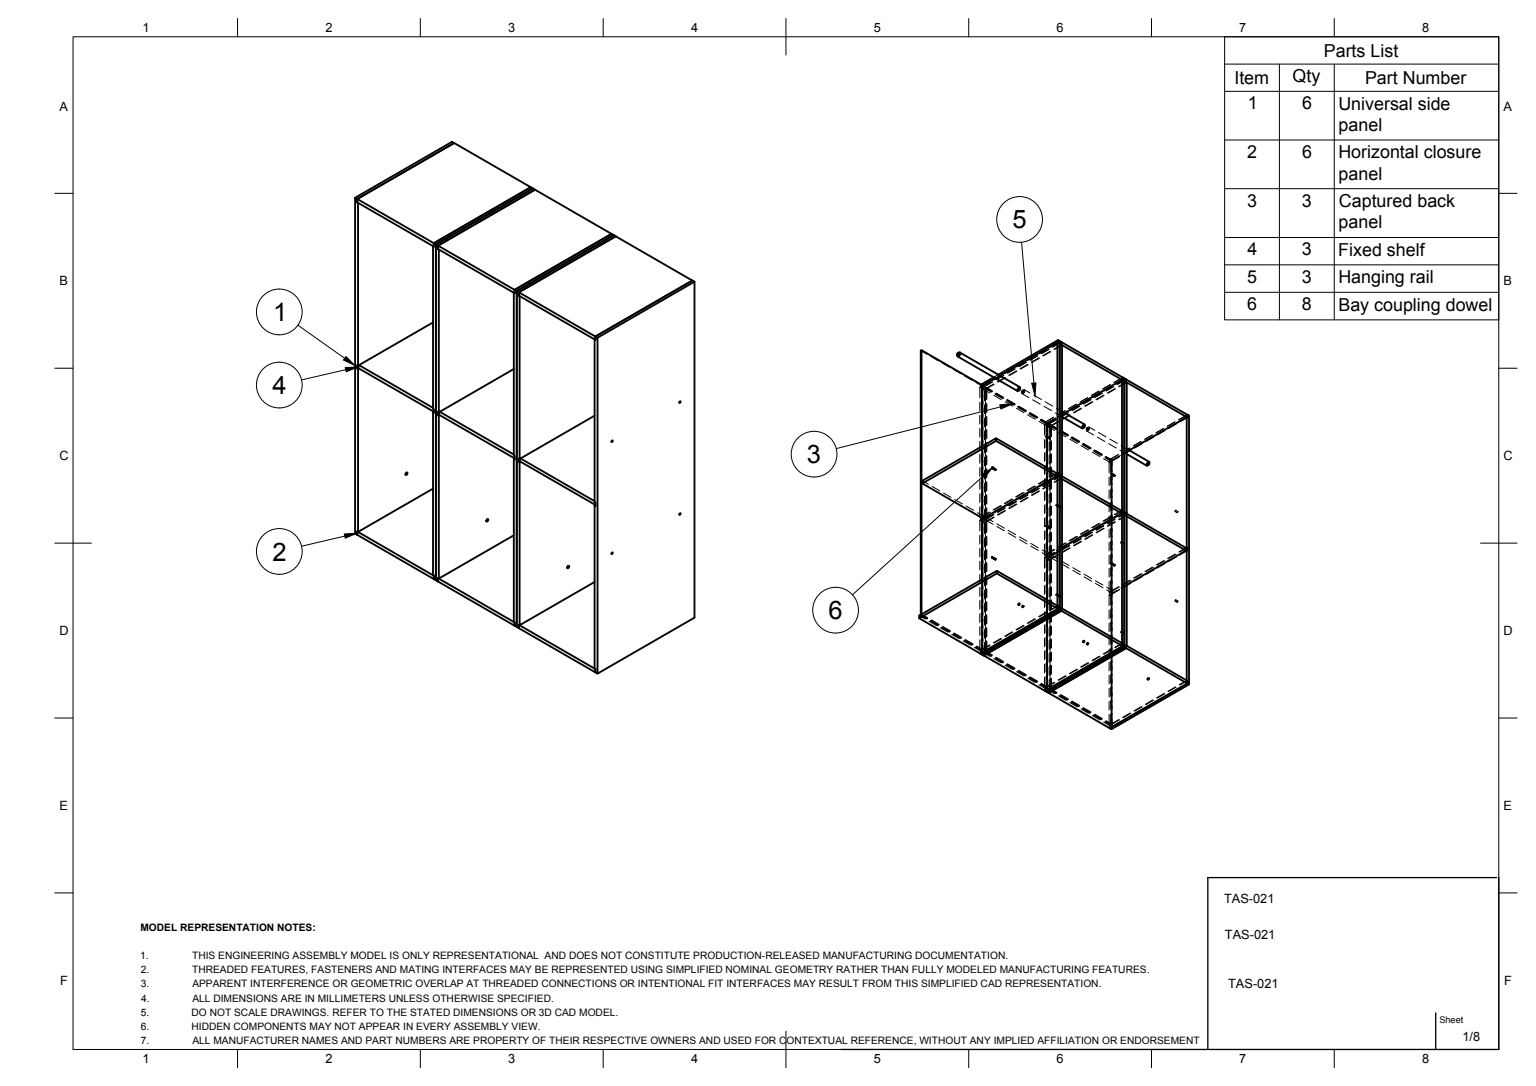
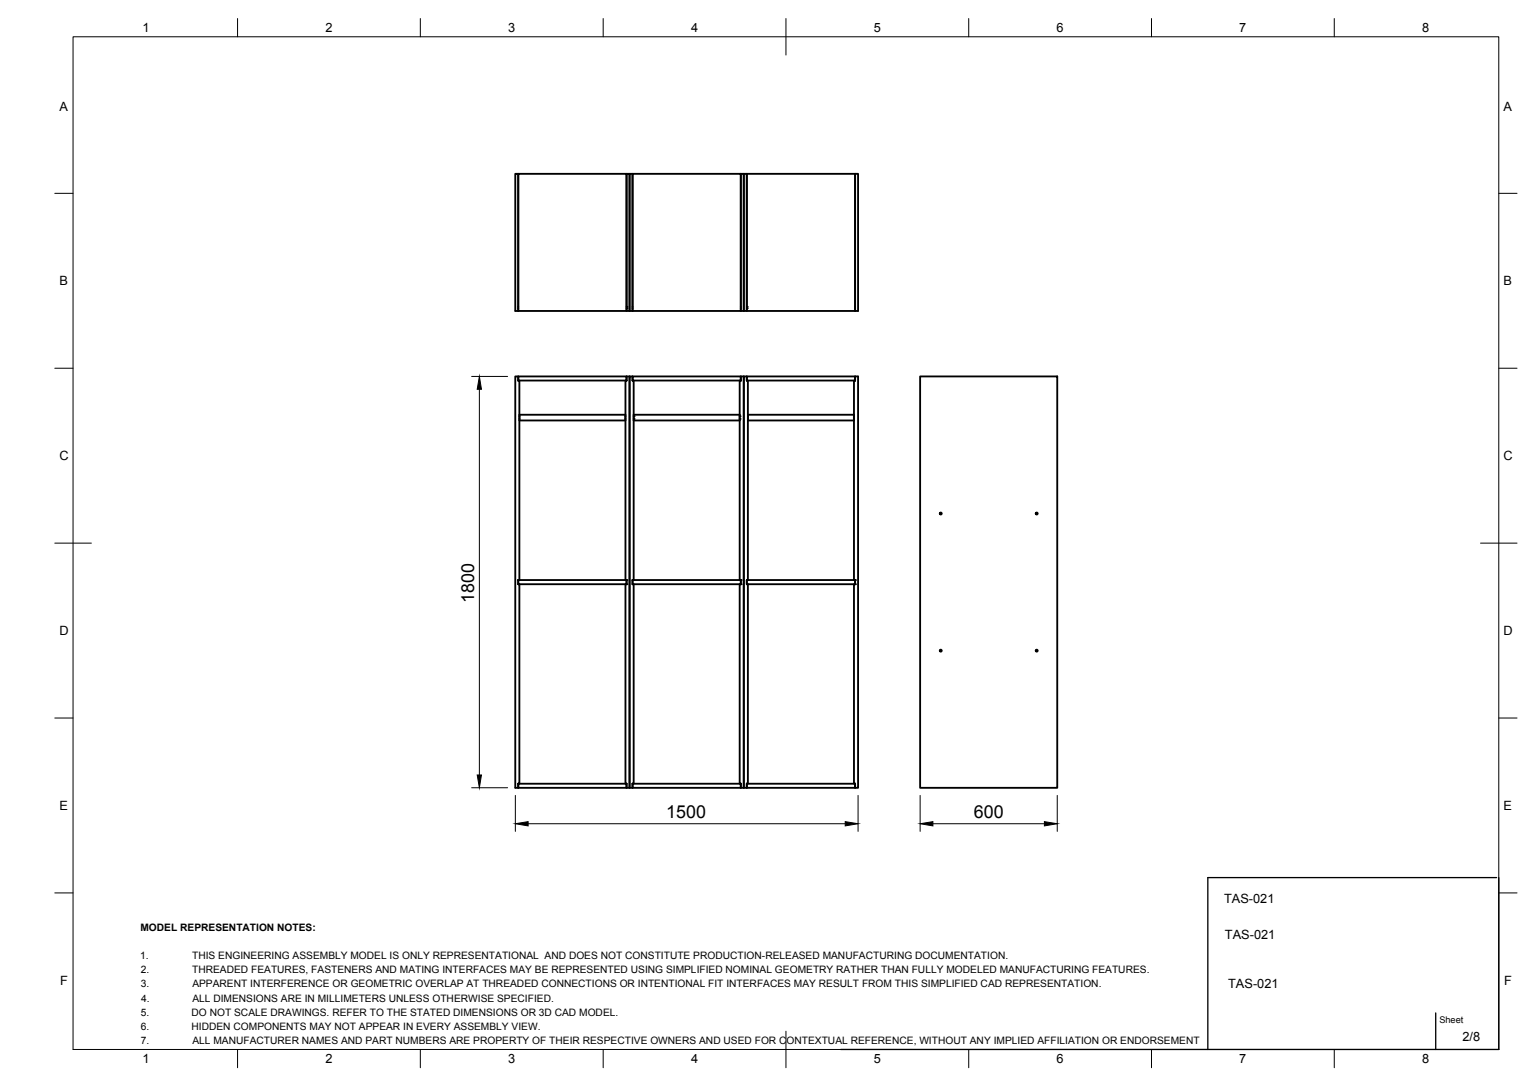
ISO-10303-21;
HEADER;
/* Generated by software containing ST-Developer
 * from STEP Tools, Inc. (www.steptools.com) 
 */

FILE_DESCRIPTION(
/* description */ (''),
/* implementation_level */ '2;1');

FILE_NAME(
/* name */ 'TAS-021.step',
/* time_stamp */ '2026-11-15T17:48:08-08:00',
/* author */ (''),
/* organization */ (''),
/* preprocessor_version */ 'ST-DEVELOPER v20.2',
/* originating_system */ 'Autodesk Translation Framework v15.17.0.0',
/* authorisation */ '');

FILE_SCHEMA (('AUTOMOTIVE_DESIGN { 1 0 10303 214 3 1 1 }'));
ENDSEC;

DATA;
#10=MECHANICAL_DESIGN_GEOMETRIC_PRESENTATION_REPRESENTATION('',(#139,#140,
#141,#142,#143,#144),#2097);
#11=ITEM_DEFINED_TRANSFORMATION($,$,#1267,#1359);
#12=ITEM_DEFINED_TRANSFORMATION($,$,#1314,#1360);
#13=ITEM_DEFINED_TRANSFORMATION($,$,#1325,#1361);
#14=ITEM_DEFINED_TRANSFORMATION($,$,#1332,#1362);
#15=ITEM_DEFINED_TRANSFORMATION($,$,#1339,#1363);
#16=ITEM_DEFINED_TRANSFORMATION($,$,#1353,#1364);
#17=ITEM_DEFINED_TRANSFORMATION($,$,#1267,#1365);
#18=ITEM_DEFINED_TRANSFORMATION($,$,#1314,#1366);
#19=ITEM_DEFINED_TRANSFORMATION($,$,#1267,#1367);
#20=ITEM_DEFINED_TRANSFORMATION($,$,#1267,#1368);
#21=ITEM_DEFINED_TRANSFORMATION($,$,#1314,#1369);
#22=ITEM_DEFINED_TRANSFORMATION($,$,#1314,#1370);
#23=ITEM_DEFINED_TRANSFORMATION($,$,#1325,#1371);
#24=ITEM_DEFINED_TRANSFORMATION($,$,#1332,#1372);
#25=ITEM_DEFINED_TRANSFORMATION($,$,#1339,#1373);
#26=ITEM_DEFINED_TRANSFORMATION($,$,#1267,#1374);
#27=ITEM_DEFINED_TRANSFORMATION($,$,#1267,#1375);
#28=ITEM_DEFINED_TRANSFORMATION($,$,#1314,#1376);
#29=ITEM_DEFINED_TRANSFORMATION($,$,#1314,#1377);
#30=ITEM_DEFINED_TRANSFORMATION($,$,#1325,#1378);
#31=ITEM_DEFINED_TRANSFORMATION($,$,#1332,#1379);
#32=ITEM_DEFINED_TRANSFORMATION($,$,#1339,#1380);
#33=ITEM_DEFINED_TRANSFORMATION($,$,#1353,#1381);
#34=ITEM_DEFINED_TRANSFORMATION($,$,#1353,#1382);
#35=ITEM_DEFINED_TRANSFORMATION($,$,#1353,#1383);
#36=ITEM_DEFINED_TRANSFORMATION($,$,#1353,#1384);
#37=ITEM_DEFINED_TRANSFORMATION($,$,#1353,#1385);
#38=ITEM_DEFINED_TRANSFORMATION($,$,#1353,#1386);
#39=ITEM_DEFINED_TRANSFORMATION($,$,#1353,#1387);
#40=(
REPRESENTATION_RELATIONSHIP($,$,#2146,#2145)
REPRESENTATION_RELATIONSHIP_WITH_TRANSFORMATION(#11)
SHAPE_REPRESENTATION_RELATIONSHIP()
);
#41=(
REPRESENTATION_RELATIONSHIP($,$,#2147,#2145)
REPRESENTATION_RELATIONSHIP_WITH_TRANSFORMATION(#12)
SHAPE_REPRESENTATION_RELATIONSHIP()
);
#42=(
REPRESENTATION_RELATIONSHIP($,$,#2148,#2145)
REPRESENTATION_RELATIONSHIP_WITH_TRANSFORMATION(#13)
SHAPE_REPRESENTATION_RELATIONSHIP()
);
#43=(
REPRESENTATION_RELATIONSHIP($,$,#2149,#2145)
REPRESENTATION_RELATIONSHIP_WITH_TRANSFORMATION(#14)
SHAPE_REPRESENTATION_RELATIONSHIP()
);
#44=(
REPRESENTATION_RELATIONSHIP($,$,#2150,#2145)
REPRESENTATION_RELATIONSHIP_WITH_TRANSFORMATION(#15)
SHAPE_REPRESENTATION_RELATIONSHIP()
);
#45=(
REPRESENTATION_RELATIONSHIP($,$,#2151,#2145)
REPRESENTATION_RELATIONSHIP_WITH_TRANSFORMATION(#16)
SHAPE_REPRESENTATION_RELATIONSHIP()
);
#46=(
REPRESENTATION_RELATIONSHIP($,$,#2146,#2145)
REPRESENTATION_RELATIONSHIP_WITH_TRANSFORMATION(#17)
SHAPE_REPRESENTATION_RELATIONSHIP()
);
#47=(
REPRESENTATION_RELATIONSHIP($,$,#2147,#2145)
REPRESENTATION_RELATIONSHIP_WITH_TRANSFORMATION(#18)
SHAPE_REPRESENTATION_RELATIONSHIP()
);
#48=(
REPRESENTATION_RELATIONSHIP($,$,#2146,#2145)
REPRESENTATION_RELATIONSHIP_WITH_TRANSFORMATION(#19)
SHAPE_REPRESENTATION_RELATIONSHIP()
);
#49=(
REPRESENTATION_RELATIONSHIP($,$,#2146,#2145)
REPRESENTATION_RELATIONSHIP_WITH_TRANSFORMATION(#20)
SHAPE_REPRESENTATION_RELATIONSHIP()
);
#50=(
REPRESENTATION_RELATIONSHIP($,$,#2147,#2145)
REPRESENTATION_RELATIONSHIP_WITH_TRANSFORMATION(#21)
SHAPE_REPRESENTATION_RELATIONSHIP()
);
#51=(
REPRESENTATION_RELATIONSHIP($,$,#2147,#2145)
REPRESENTATION_RELATIONSHIP_WITH_TRANSFORMATION(#22)
SHAPE_REPRESENTATION_RELATIONSHIP()
);
#52=(
REPRESENTATION_RELATIONSHIP($,$,#2148,#2145)
REPRESENTATION_RELATIONSHIP_WITH_TRANSFORMATION(#23)
SHAPE_REPRESENTATION_RELATIONSHIP()
);
#53=(
REPRESENTATION_RELATIONSHIP($,$,#2149,#2145)
REPRESENTATION_RELATIONSHIP_WITH_TRANSFORMATION(#24)
SHAPE_REPRESENTATION_RELATIONSHIP()
);
#54=(
REPRESENTATION_RELATIONSHIP($,$,#2150,#2145)
REPRESENTATION_RELATIONSHIP_WITH_TRANSFORMATION(#25)
SHAPE_REPRESENTATION_RELATIONSHIP()
);
#55=(
REPRESENTATION_RELATIONSHIP($,$,#2146,#2145)
REPRESENTATION_RELATIONSHIP_WITH_TRANSFORMATION(#26)
SHAPE_REPRESENTATION_RELATIONSHIP()
);
#56=(
REPRESENTATION_RELATIONSHIP($,$,#2146,#2145)
REPRESENTATION_RELATIONSHIP_WITH_TRANSFORMATION(#27)
SHAPE_REPRESENTATION_RELATIONSHIP()
);
#57=(
REPRESENTATION_RELATIONSHIP($,$,#2147,#2145)
REPRESENTATION_RELATIONSHIP_WITH_TRANSFORMATION(#28)
SHAPE_REPRESENTATION_RELATIONSHIP()
);
#58=(
REPRESENTATION_RELATIONSHIP($,$,#2147,#2145)
REPRESENTATION_RELATIONSHIP_WITH_TRANSFORMATION(#29)
SHAPE_REPRESENTATION_RELATIONSHIP()
);
#59=(
REPRESENTATION_RELATIONSHIP($,$,#2148,#2145)
REPRESENTATION_RELATIONSHIP_WITH_TRANSFORMATION(#30)
SHAPE_REPRESENTATION_RELATIONSHIP()
);
#60=(
REPRESENTATION_RELATIONSHIP($,$,#2149,#2145)
REPRESENTATION_RELATIONSHIP_WITH_TRANSFORMATION(#31)
SHAPE_REPRESENTATION_RELATIONSHIP()
);
#61=(
REPRESENTATION_RELATIONSHIP($,$,#2150,#2145)
REPRESENTATION_RELATIONSHIP_WITH_TRANSFORMATION(#32)
SHAPE_REPRESENTATION_RELATIONSHIP()
);
#62=(
REPRESENTATION_RELATIONSHIP($,$,#2151,#2145)
REPRESENTATION_RELATIONSHIP_WITH_TRANSFORMATION(#33)
SHAPE_REPRESENTATION_RELATIONSHIP()
);
#63=(
REPRESENTATION_RELATIONSHIP($,$,#2151,#2145)
REPRESENTATION_RELATIONSHIP_WITH_TRANSFORMATION(#34)
SHAPE_REPRESENTATION_RELATIONSHIP()
);
#64=(
REPRESENTATION_RELATIONSHIP($,$,#2151,#2145)
REPRESENTATION_RELATIONSHIP_WITH_TRANSFORMATION(#35)
SHAPE_REPRESENTATION_RELATIONSHIP()
);
#65=(
REPRESENTATION_RELATIONSHIP($,$,#2151,#2145)
REPRESENTATION_RELATIONSHIP_WITH_TRANSFORMATION(#36)
SHAPE_REPRESENTATION_RELATIONSHIP()
);
#66=(
REPRESENTATION_RELATIONSHIP($,$,#2151,#2145)
REPRESENTATION_RELATIONSHIP_WITH_TRANSFORMATION(#37)
SHAPE_REPRESENTATION_RELATIONSHIP()
);
#67=(
REPRESENTATION_RELATIONSHIP($,$,#2151,#2145)
REPRESENTATION_RELATIONSHIP_WITH_TRANSFORMATION(#38)
SHAPE_REPRESENTATION_RELATIONSHIP()
);
#68=(
REPRESENTATION_RELATIONSHIP($,$,#2151,#2145)
REPRESENTATION_RELATIONSHIP_WITH_TRANSFORMATION(#39)
SHAPE_REPRESENTATION_RELATIONSHIP()
);
#69=CONTEXT_DEPENDENT_SHAPE_REPRESENTATION(#40,#2116);
#70=CONTEXT_DEPENDENT_SHAPE_REPRESENTATION(#41,#2117);
#71=CONTEXT_DEPENDENT_SHAPE_REPRESENTATION(#42,#2118);
#72=CONTEXT_DEPENDENT_SHAPE_REPRESENTATION(#43,#2119);
#73=CONTEXT_DEPENDENT_SHAPE_REPRESENTATION(#44,#2120);
#74=CONTEXT_DEPENDENT_SHAPE_REPRESENTATION(#45,#2121);
#75=CONTEXT_DEPENDENT_SHAPE_REPRESENTATION(#46,#2122);
#76=CONTEXT_DEPENDENT_SHAPE_REPRESENTATION(#47,#2123);
#77=CONTEXT_DEPENDENT_SHAPE_REPRESENTATION(#48,#2124);
#78=CONTEXT_DEPENDENT_SHAPE_REPRESENTATION(#49,#2125);
#79=CONTEXT_DEPENDENT_SHAPE_REPRESENTATION(#50,#2126);
#80=CONTEXT_DEPENDENT_SHAPE_REPRESENTATION(#51,#2127);
#81=CONTEXT_DEPENDENT_SHAPE_REPRESENTATION(#52,#2128);
#82=CONTEXT_DEPENDENT_SHAPE_REPRESENTATION(#53,#2129);
#83=CONTEXT_DEPENDENT_SHAPE_REPRESENTATION(#54,#2130);
#84=CONTEXT_DEPENDENT_SHAPE_REPRESENTATION(#55,#2131);
#85=CONTEXT_DEPENDENT_SHAPE_REPRESENTATION(#56,#2132);
#86=CONTEXT_DEPENDENT_SHAPE_REPRESENTATION(#57,#2133);
#87=CONTEXT_DEPENDENT_SHAPE_REPRESENTATION(#58,#2134);
#88=CONTEXT_DEPENDENT_SHAPE_REPRESENTATION(#59,#2135);
#89=CONTEXT_DEPENDENT_SHAPE_REPRESENTATION(#60,#2136);
#90=CONTEXT_DEPENDENT_SHAPE_REPRESENTATION(#61,#2137);
#91=CONTEXT_DEPENDENT_SHAPE_REPRESENTATION(#62,#2138);
#92=CONTEXT_DEPENDENT_SHAPE_REPRESENTATION(#63,#2139);
#93=CONTEXT_DEPENDENT_SHAPE_REPRESENTATION(#64,#2140);
#94=CONTEXT_DEPENDENT_SHAPE_REPRESENTATION(#65,#2141);
#95=CONTEXT_DEPENDENT_SHAPE_REPRESENTATION(#66,#2142);
#96=CONTEXT_DEPENDENT_SHAPE_REPRESENTATION(#67,#2143);
#97=CONTEXT_DEPENDENT_SHAPE_REPRESENTATION(#68,#2144);
#98=NEXT_ASSEMBLY_USAGE_OCCURRENCE('Universal side panel:1',
'Universal side panel:1','Universal side panel:1',#2153,#2154,
'Universal side panel:1');
#99=NEXT_ASSEMBLY_USAGE_OCCURRENCE('Horizontal closure panel:1',
'Horizontal closure panel:1','Horizontal closure panel:1',#2153,#2155,
'Horizontal closure panel:1');
#100=NEXT_ASSEMBLY_USAGE_OCCURRENCE('Captured back panel:1',
'Captured back panel:1','Captured back panel:1',#2153,#2156,
'Captured back panel:1');
#101=NEXT_ASSEMBLY_USAGE_OCCURRENCE('Fixed shelf:1','Fixed shelf:1',
'Fixed shelf:1',#2153,#2157,'Fixed shelf:1');
#102=NEXT_ASSEMBLY_USAGE_OCCURRENCE('Hanging rail:1','Hanging rail:1',
'Hanging rail:1',#2153,#2158,'Hanging rail:1');
#103=NEXT_ASSEMBLY_USAGE_OCCURRENCE('Bay coupling dowel:1',
'Bay coupling dowel:1','Bay coupling dowel:1',#2153,#2159,
'Bay coupling dowel:1');
#104=NEXT_ASSEMBLY_USAGE_OCCURRENCE('Universal side panel:2',
'Universal side panel:2','Universal side panel:2',#2153,#2154,
'Universal side panel:2');
#105=NEXT_ASSEMBLY_USAGE_OCCURRENCE('Horizontal closure panel:2',
'Horizontal closure panel:2','Horizontal closure panel:2',#2153,#2155,
'Horizontal closure panel:2');
#106=NEXT_ASSEMBLY_USAGE_OCCURRENCE('Universal side panel:3',
'Universal side panel:3','Universal side panel:3',#2153,#2154,
'Universal side panel:3');
#107=NEXT_ASSEMBLY_USAGE_OCCURRENCE('Universal side panel:4',
'Universal side panel:4','Universal side panel:4',#2153,#2154,
'Universal side panel:4');
#108=NEXT_ASSEMBLY_USAGE_OCCURRENCE('Horizontal closure panel:3',
'Horizontal closure panel:3','Horizontal closure panel:3',#2153,#2155,
'Horizontal closure panel:3');
#109=NEXT_ASSEMBLY_USAGE_OCCURRENCE('Horizontal closure panel:4',
'Horizontal closure panel:4','Horizontal closure panel:4',#2153,#2155,
'Horizontal closure panel:4');
#110=NEXT_ASSEMBLY_USAGE_OCCURRENCE('Captured back panel:2',
'Captured back panel:2','Captured back panel:2',#2153,#2156,
'Captured back panel:2');
#111=NEXT_ASSEMBLY_USAGE_OCCURRENCE('Fixed shelf:2','Fixed shelf:2',
'Fixed shelf:2',#2153,#2157,'Fixed shelf:2');
#112=NEXT_ASSEMBLY_USAGE_OCCURRENCE('Hanging rail:2','Hanging rail:2',
'Hanging rail:2',#2153,#2158,'Hanging rail:2');
#113=NEXT_ASSEMBLY_USAGE_OCCURRENCE('Universal side panel:5',
'Universal side panel:5','Universal side panel:5',#2153,#2154,
'Universal side panel:5');
#114=NEXT_ASSEMBLY_USAGE_OCCURRENCE('Universal side panel:6',
'Universal side panel:6','Universal side panel:6',#2153,#2154,
'Universal side panel:6');
#115=NEXT_ASSEMBLY_USAGE_OCCURRENCE('Horizontal closure panel:5',
'Horizontal closure panel:5','Horizontal closure panel:5',#2153,#2155,
'Horizontal closure panel:5');
#116=NEXT_ASSEMBLY_USAGE_OCCURRENCE('Horizontal closure panel:6',
'Horizontal closure panel:6','Horizontal closure panel:6',#2153,#2155,
'Horizontal closure panel:6');
#117=NEXT_ASSEMBLY_USAGE_OCCURRENCE('Captured back panel:3',
'Captured back panel:3','Captured back panel:3',#2153,#2156,
'Captured back panel:3');
#118=NEXT_ASSEMBLY_USAGE_OCCURRENCE('Fixed shelf:3','Fixed shelf:3',
'Fixed shelf:3',#2153,#2157,'Fixed shelf:3');
#119=NEXT_ASSEMBLY_USAGE_OCCURRENCE('Hanging rail:3','Hanging rail:3',
'Hanging rail:3',#2153,#2158,'Hanging rail:3');
#120=NEXT_ASSEMBLY_USAGE_OCCURRENCE('Bay coupling dowel:2',
'Bay coupling dowel:2','Bay coupling dowel:2',#2153,#2159,
'Bay coupling dowel:2');
#121=NEXT_ASSEMBLY_USAGE_OCCURRENCE('Bay coupling dowel:3',
'Bay coupling dowel:3','Bay coupling dowel:3',#2153,#2159,
'Bay coupling dowel:3');
#122=NEXT_ASSEMBLY_USAGE_OCCURRENCE('Bay coupling dowel:4',
'Bay coupling dowel:4','Bay coupling dowel:4',#2153,#2159,
'Bay coupling dowel:4');
#123=NEXT_ASSEMBLY_USAGE_OCCURRENCE('Bay coupling dowel:5',
'Bay coupling dowel:5','Bay coupling dowel:5',#2153,#2159,
'Bay coupling dowel:5');
#124=NEXT_ASSEMBLY_USAGE_OCCURRENCE('Bay coupling dowel:6',
'Bay coupling dowel:6','Bay coupling dowel:6',#2153,#2159,
'Bay coupling dowel:6');
#125=NEXT_ASSEMBLY_USAGE_OCCURRENCE('Bay coupling dowel:7',
'Bay coupling dowel:7','Bay coupling dowel:7',#2153,#2159,
'Bay coupling dowel:7');
#126=NEXT_ASSEMBLY_USAGE_OCCURRENCE('Bay coupling dowel:8',
'Bay coupling dowel:8','Bay coupling dowel:8',#2153,#2159,
'Bay coupling dowel:8');
#127=SHAPE_REPRESENTATION_RELATIONSHIP('SRR','None',#2146,#133);
#128=SHAPE_REPRESENTATION_RELATIONSHIP('SRR','None',#2147,#134);
#129=SHAPE_REPRESENTATION_RELATIONSHIP('SRR','None',#2148,#135);
#130=SHAPE_REPRESENTATION_RELATIONSHIP('SRR','None',#2149,#136);
#131=SHAPE_REPRESENTATION_RELATIONSHIP('SRR','None',#2150,#137);
#132=SHAPE_REPRESENTATION_RELATIONSHIP('SRR','None',#2151,#138);
#133=ADVANCED_BREP_SHAPE_REPRESENTATION('',(#145),#2091);
#134=ADVANCED_BREP_SHAPE_REPRESENTATION('',(#146),#2092);
#135=ADVANCED_BREP_SHAPE_REPRESENTATION('',(#147),#2093);
#136=ADVANCED_BREP_SHAPE_REPRESENTATION('',(#148),#2094);
#137=ADVANCED_BREP_SHAPE_REPRESENTATION('',(#149),#2095);
#138=ADVANCED_BREP_SHAPE_REPRESENTATION('',(#150),#2096);
#139=STYLED_ITEM('',(#2185),#145);
#140=STYLED_ITEM('',(#2186),#146);
#141=STYLED_ITEM('',(#2187),#147);
#142=STYLED_ITEM('',(#2188),#148);
#143=STYLED_ITEM('',(#2189),#149);
#144=STYLED_ITEM('',(#2190),#150);
#145=MANIFOLD_SOLID_BREP('Body1',#1193);
#146=MANIFOLD_SOLID_BREP('Body1',#1194);
#147=MANIFOLD_SOLID_BREP('Body1',#1195);
#148=MANIFOLD_SOLID_BREP('Body1',#1196);
#149=MANIFOLD_SOLID_BREP('Body1',#1197);
#150=MANIFOLD_SOLID_BREP('Body1',#1198);
#151=FACE_BOUND('',#301,.T.);
#152=FACE_BOUND('',#308,.T.);
#153=FACE_BOUND('',#316,.T.);
#154=FACE_BOUND('',#317,.T.);
#155=FACE_BOUND('',#318,.T.);
#156=FACE_BOUND('',#319,.T.);
#157=FACE_BOUND('',#349,.T.);
#158=FACE_BOUND('',#351,.T.);
#159=PLANE('',#1271);
#160=PLANE('',#1275);
#161=PLANE('',#1279);
#162=PLANE('',#1283);
#163=PLANE('',#1287);
#164=PLANE('',#1291);
#165=PLANE('',#1292);
#166=PLANE('',#1293);
#167=PLANE('',#1294);
#168=PLANE('',#1295);
#169=PLANE('',#1296);
#170=PLANE('',#1297);
#171=PLANE('',#1298);
#172=PLANE('',#1299);
#173=PLANE('',#1300);
#174=PLANE('',#1301);
#175=PLANE('',#1302);
#176=PLANE('',#1303);
#177=PLANE('',#1304);
#178=PLANE('',#1305);
#179=PLANE('',#1306);
#180=PLANE('',#1307);
#181=PLANE('',#1308);
#182=PLANE('',#1309);
#183=PLANE('',#1310);
#184=PLANE('',#1311);
#185=PLANE('',#1312);
#186=PLANE('',#1313);
#187=PLANE('',#1315);
#188=PLANE('',#1316);
#189=PLANE('',#1317);
#190=PLANE('',#1318);
#191=PLANE('',#1319);
#192=PLANE('',#1320);
#193=PLANE('',#1321);
#194=PLANE('',#1322);
#195=PLANE('',#1323);
#196=PLANE('',#1324);
#197=PLANE('',#1326);
#198=PLANE('',#1327);
#199=PLANE('',#1328);
#200=PLANE('',#1329);
#201=PLANE('',#1330);
#202=PLANE('',#1331);
#203=PLANE('',#1333);
#204=PLANE('',#1334);
#205=PLANE('',#1335);
#206=PLANE('',#1336);
#207=PLANE('',#1337);
#208=PLANE('',#1338);
#209=PLANE('',#1343);
#210=PLANE('',#1347);
#211=PLANE('',#1351);
#212=PLANE('',#1352);
#213=PLANE('',#1357);
#214=PLANE('',#1358);
#215=FACE_OUTER_BOUND('',#281,.T.);
#216=FACE_OUTER_BOUND('',#282,.T.);
#217=FACE_OUTER_BOUND('',#283,.T.);
#218=FACE_OUTER_BOUND('',#284,.T.);
#219=FACE_OUTER_BOUND('',#285,.T.);
#220=FACE_OUTER_BOUND('',#286,.T.);
#221=FACE_OUTER_BOUND('',#287,.T.);
#222=FACE_OUTER_BOUND('',#288,.T.);
#223=FACE_OUTER_BOUND('',#289,.T.);
#224=FACE_OUTER_BOUND('',#290,.T.);
#225=FACE_OUTER_BOUND('',#291,.T.);
#226=FACE_OUTER_BOUND('',#292,.T.);
#227=FACE_OUTER_BOUND('',#293,.T.);
#228=FACE_OUTER_BOUND('',#294,.T.);
#229=FACE_OUTER_BOUND('',#295,.T.);
#230=FACE_OUTER_BOUND('',#296,.T.);
#231=FACE_OUTER_BOUND('',#297,.T.);
#232=FACE_OUTER_BOUND('',#298,.T.);
#233=FACE_OUTER_BOUND('',#299,.T.);
#234=FACE_OUTER_BOUND('',#300,.T.);
#235=FACE_OUTER_BOUND('',#302,.T.);
#236=FACE_OUTER_BOUND('',#303,.T.);
#237=FACE_OUTER_BOUND('',#304,.T.);
#238=FACE_OUTER_BOUND('',#305,.T.);
#239=FACE_OUTER_BOUND('',#306,.T.);
#240=FACE_OUTER_BOUND('',#307,.T.);
#241=FACE_OUTER_BOUND('',#309,.T.);
#242=FACE_OUTER_BOUND('',#310,.T.);
#243=FACE_OUTER_BOUND('',#311,.T.);
#244=FACE_OUTER_BOUND('',#312,.T.);
#245=FACE_OUTER_BOUND('',#313,.T.);
#246=FACE_OUTER_BOUND('',#314,.T.);
#247=FACE_OUTER_BOUND('',#315,.T.);
#248=FACE_OUTER_BOUND('',#320,.T.);
#249=FACE_OUTER_BOUND('',#321,.T.);
#250=FACE_OUTER_BOUND('',#322,.T.);
#251=FACE_OUTER_BOUND('',#323,.T.);
#252=FACE_OUTER_BOUND('',#324,.T.);
#253=FACE_OUTER_BOUND('',#325,.T.);
#254=FACE_OUTER_BOUND('',#326,.T.);
#255=FACE_OUTER_BOUND('',#327,.T.);
#256=FACE_OUTER_BOUND('',#328,.T.);
#257=FACE_OUTER_BOUND('',#329,.T.);
#258=FACE_OUTER_BOUND('',#330,.T.);
#259=FACE_OUTER_BOUND('',#331,.T.);
#260=FACE_OUTER_BOUND('',#332,.T.);
#261=FACE_OUTER_BOUND('',#333,.T.);
#262=FACE_OUTER_BOUND('',#334,.T.);
#263=FACE_OUTER_BOUND('',#335,.T.);
#264=FACE_OUTER_BOUND('',#336,.T.);
#265=FACE_OUTER_BOUND('',#337,.T.);
#266=FACE_OUTER_BOUND('',#338,.T.);
#267=FACE_OUTER_BOUND('',#339,.T.);
#268=FACE_OUTER_BOUND('',#340,.T.);
#269=FACE_OUTER_BOUND('',#341,.T.);
#270=FACE_OUTER_BOUND('',#342,.T.);
#271=FACE_OUTER_BOUND('',#343,.T.);
#272=FACE_OUTER_BOUND('',#344,.T.);
#273=FACE_OUTER_BOUND('',#345,.T.);
#274=FACE_OUTER_BOUND('',#346,.T.);
#275=FACE_OUTER_BOUND('',#347,.T.);
#276=FACE_OUTER_BOUND('',#348,.T.);
#277=FACE_OUTER_BOUND('',#350,.T.);
#278=FACE_OUTER_BOUND('',#352,.T.);
#279=FACE_OUTER_BOUND('',#353,.T.);
#280=FACE_OUTER_BOUND('',#354,.T.);
#281=EDGE_LOOP('',(#841,#842,#843,#844));
#282=EDGE_LOOP('',(#845));
#283=EDGE_LOOP('',(#846,#847,#848,#849));
#284=EDGE_LOOP('',(#850));
#285=EDGE_LOOP('',(#851,#852,#853,#854));
#286=EDGE_LOOP('',(#855));
#287=EDGE_LOOP('',(#856,#857,#858,#859));
#288=EDGE_LOOP('',(#860));
#289=EDGE_LOOP('',(#861,#862,#863,#864));
#290=EDGE_LOOP('',(#865));
#291=EDGE_LOOP('',(#866,#867,#868,#869));
#292=EDGE_LOOP('',(#870));
#293=EDGE_LOOP('',(#871,#872,#873,#874));
#294=EDGE_LOOP('',(#875,#876,#877,#878));
#295=EDGE_LOOP('',(#879,#880,#881,#882));
#296=EDGE_LOOP('',(#883,#884,#885,#886));
#297=EDGE_LOOP('',(#887,#888,#889,#890,#891,#892,#893,#894,#895,#896,#897,
#898,#899,#900,#901,#902,#903,#904,#905,#906));
#298=EDGE_LOOP('',(#907,#908,#909,#910));
#299=EDGE_LOOP('',(#911,#912,#913,#914));
#300=EDGE_LOOP('',(#915,#916,#917,#918));
#301=EDGE_LOOP('',(#919));
#302=EDGE_LOOP('',(#920,#921,#922,#923));
#303=EDGE_LOOP('',(#924,#925,#926,#927));
#304=EDGE_LOOP('',(#928,#929,#930,#931));
#305=EDGE_LOOP('',(#932,#933,#934,#935));
#306=EDGE_LOOP('',(#936,#937,#938,#939));
#307=EDGE_LOOP('',(#940,#941,#942,#943));
#308=EDGE_LOOP('',(#944));
#309=EDGE_LOOP('',(#945,#946,#947,#948));
#310=EDGE_LOOP('',(#949,#950,#951,#952));
#311=EDGE_LOOP('',(#953,#954,#955,#956));
#312=EDGE_LOOP('',(#957,#958,#959,#960,#961,#962,#963,#964,#965,#966,#967,
#968));
#313=EDGE_LOOP('',(#969,#970,#971,#972));
#314=EDGE_LOOP('',(#973,#974,#975,#976,#977,#978,#979,#980,#981,#982,#983,
#984));
#315=EDGE_LOOP('',(#985,#986,#987,#988));
#316=EDGE_LOOP('',(#989));
#317=EDGE_LOOP('',(#990));
#318=EDGE_LOOP('',(#991));
#319=EDGE_LOOP('',(#992));
#320=EDGE_LOOP('',(#993,#994,#995,#996));
#321=EDGE_LOOP('',(#997,#998,#999,#1000));
#322=EDGE_LOOP('',(#1001,#1002,#1003,#1004));
#323=EDGE_LOOP('',(#1005,#1006,#1007,#1008));
#324=EDGE_LOOP('',(#1009,#1010,#1011,#1012,#1013,#1014,#1015,#1016));
#325=EDGE_LOOP('',(#1017,#1018,#1019,#1020));
#326=EDGE_LOOP('',(#1021,#1022,#1023,#1024));
#327=EDGE_LOOP('',(#1025,#1026,#1027,#1028));
#328=EDGE_LOOP('',(#1029,#1030,#1031,#1032,#1033,#1034,#1035,#1036));
#329=EDGE_LOOP('',(#1037,#1038,#1039,#1040));
#330=EDGE_LOOP('',(#1041,#1042,#1043,#1044));
#331=EDGE_LOOP('',(#1045,#1046,#1047,#1048));
#332=EDGE_LOOP('',(#1049,#1050,#1051,#1052));
#333=EDGE_LOOP('',(#1053,#1054,#1055,#1056));
#334=EDGE_LOOP('',(#1057,#1058,#1059,#1060));
#335=EDGE_LOOP('',(#1061,#1062,#1063,#1064));
#336=EDGE_LOOP('',(#1065,#1066,#1067,#1068));
#337=EDGE_LOOP('',(#1069,#1070,#1071,#1072));
#338=EDGE_LOOP('',(#1073,#1074,#1075,#1076));
#339=EDGE_LOOP('',(#1077,#1078,#1079,#1080));
#340=EDGE_LOOP('',(#1081,#1082,#1083,#1084));
#341=EDGE_LOOP('',(#1085,#1086,#1087,#1088));
#342=EDGE_LOOP('',(#1089,#1090,#1091,#1092));
#343=EDGE_LOOP('',(#1093,#1094,#1095,#1096));
#344=EDGE_LOOP('',(#1097));
#345=EDGE_LOOP('',(#1098,#1099,#1100,#1101));
#346=EDGE_LOOP('',(#1102));
#347=EDGE_LOOP('',(#1103,#1104,#1105,#1106));
#348=EDGE_LOOP('',(#1107));
#349=EDGE_LOOP('',(#1108));
#350=EDGE_LOOP('',(#1109));
#351=EDGE_LOOP('',(#1110));
#352=EDGE_LOOP('',(#1111,#1112,#1113,#1114));
#353=EDGE_LOOP('',(#1115));
#354=EDGE_LOOP('',(#1116));
#355=LINE('',#1756,#473);
#356=LINE('',#1763,#474);
#357=LINE('',#1770,#475);
#358=LINE('',#1777,#476);
#359=LINE('',#1784,#477);
#360=LINE('',#1791,#478);
#361=LINE('',#1797,#479);
#362=LINE('',#1799,#480);
#363=LINE('',#1801,#481);
#364=LINE('',#1802,#482);
#365=LINE('',#1806,#483);
#366=LINE('',#1808,#484);
#367=LINE('',#1810,#485);
#368=LINE('',#1811,#486);
#369=LINE('',#1815,#487);
#370=LINE('',#1817,#488);
#371=LINE('',#1819,#489);
#372=LINE('',#1820,#490);
#373=LINE('',#1824,#491);
#374=LINE('',#1826,#492);
#375=LINE('',#1828,#493);
#376=LINE('',#1829,#494);
#377=LINE('',#1832,#495);
#378=LINE('',#1834,#496);
#379=LINE('',#1836,#497);
#380=LINE('',#1838,#498);
#381=LINE('',#1839,#499);
#382=LINE('',#1841,#500);
#383=LINE('',#1843,#501);
#384=LINE('',#1844,#502);
#385=LINE('',#1846,#503);
#386=LINE('',#1848,#504);
#387=LINE('',#1850,#505);
#388=LINE('',#1852,#506);
#389=LINE('',#1853,#507);
#390=LINE('',#1855,#508);
#391=LINE('',#1857,#509);
#392=LINE('',#1858,#510);
#393=LINE('',#1861,#511);
#394=LINE('',#1862,#512);
#395=LINE('',#1865,#513);
#396=LINE('',#1866,#514);
#397=LINE('',#1869,#515);
#398=LINE('',#1870,#516);
#399=LINE('',#1873,#517);
#400=LINE('',#1874,#518);
#401=LINE('',#1876,#519);
#402=LINE('',#1878,#520);
#403=LINE('',#1881,#521);
#404=LINE('',#1882,#522);
#405=LINE('',#1885,#523);
#406=LINE('',#1886,#524);
#407=LINE('',#1889,#525);
#408=LINE('',#1890,#526);
#409=LINE('',#1893,#527);
#410=LINE('',#1894,#528);
#411=LINE('',#1896,#529);
#412=LINE('',#1898,#530);
#413=LINE('',#1901,#531);
#414=LINE('',#1903,#532);
#415=LINE('',#1904,#533);
#416=LINE('',#1907,#534);
#417=LINE('',#1908,#535);
#418=LINE('',#1911,#536);
#419=LINE('',#1912,#537);
#420=LINE('',#1914,#538);
#421=LINE('',#1920,#539);
#422=LINE('',#1922,#540);
#423=LINE('',#1924,#541);
#424=LINE('',#1925,#542);
#425=LINE('',#1929,#543);
#426=LINE('',#1931,#544);
#427=LINE('',#1933,#545);
#428=LINE('',#1934,#546);
#429=LINE('',#1936,#547);
#430=LINE('',#1937,#548);
#431=LINE('',#1940,#549);
#432=LINE('',#1942,#550);
#433=LINE('',#1944,#551);
#434=LINE('',#1946,#552);
#435=LINE('',#1947,#553);
#436=LINE('',#1950,#554);
#437=LINE('',#1951,#555);
#438=LINE('',#1954,#556);
#439=LINE('',#1956,#557);
#440=LINE('',#1957,#558);
#441=LINE('',#1960,#559);
#442=LINE('',#1961,#560);
#443=LINE('',#1963,#561);
#444=LINE('',#1964,#562);
#445=LINE('',#1971,#563);
#446=LINE('',#1973,#564);
#447=LINE('',#1975,#565);
#448=LINE('',#1976,#566);
#449=LINE('',#1979,#567);
#450=LINE('',#1981,#568);
#451=LINE('',#1982,#569);
#452=LINE('',#1985,#570);
#453=LINE('',#1987,#571);
#454=LINE('',#1988,#572);
#455=LINE('',#1990,#573);
#456=LINE('',#1991,#574);
#457=LINE('',#1998,#575);
#458=LINE('',#2000,#576);
#459=LINE('',#2002,#577);
#460=LINE('',#2003,#578);
#461=LINE('',#2006,#579);
#462=LINE('',#2008,#580);
#463=LINE('',#2009,#581);
#464=LINE('',#2012,#582);
#465=LINE('',#2014,#583);
#466=LINE('',#2015,#584);
#467=LINE('',#2017,#585);
#468=LINE('',#2018,#586);
#469=LINE('',#2026,#587);
#470=LINE('',#2033,#588);
#471=LINE('',#2040,#589);
#472=LINE('',#2049,#590);
#473=VECTOR('',#1396,0.409999999999997);
#474=VECTOR('',#1405,0.409999999999997);
#475=VECTOR('',#1414,0.409999999999997);
#476=VECTOR('',#1423,0.409999999999997);
#477=VECTOR('',#1432,0.620000000000001);
#478=VECTOR('',#1441,0.620000000000005);
#479=VECTOR('',#1448,1.);
#480=VECTOR('',#1449,1.);
#481=VECTOR('',#1450,1.);
#482=VECTOR('',#1451,1.);
#483=VECTOR('',#1454,1.);
#484=VECTOR('',#1455,1.);
#485=VECTOR('',#1456,1.);
#486=VECTOR('',#1457,1.);
#487=VECTOR('',#1460,1.);
#488=VECTOR('',#1461,1.);
#489=VECTOR('',#1462,1.);
#490=VECTOR('',#1463,1.);
#491=VECTOR('',#1466,1.);
#492=VECTOR('',#1467,1.);
#493=VECTOR('',#1468,1.);
#494=VECTOR('',#1469,1.);
#495=VECTOR('',#1472,1.);
#496=VECTOR('',#1473,1.);
#497=VECTOR('',#1474,1.);
#498=VECTOR('',#1475,1.);
#499=VECTOR('',#1476,1.);
#500=VECTOR('',#1477,1.);
#501=VECTOR('',#1478,1.);
#502=VECTOR('',#1479,1.);
#503=VECTOR('',#1480,1.);
#504=VECTOR('',#1481,1.);
#505=VECTOR('',#1482,1.);
#506=VECTOR('',#1483,1.);
#507=VECTOR('',#1484,1.);
#508=VECTOR('',#1485,1.);
#509=VECTOR('',#1486,1.);
#510=VECTOR('',#1487,1.);
#511=VECTOR('',#1490,1.);
#512=VECTOR('',#1491,1.);
#513=VECTOR('',#1494,1.);
#514=VECTOR('',#1495,1.);
#515=VECTOR('',#1498,1.);
#516=VECTOR('',#1499,1.);
#517=VECTOR('',#1502,1.);
#518=VECTOR('',#1503,1.);
#519=VECTOR('',#1506,1.);
#520=VECTOR('',#1509,1.);
#521=VECTOR('',#1512,1.);
#522=VECTOR('',#1513,1.);
#523=VECTOR('',#1516,1.);
#524=VECTOR('',#1517,1.);
#525=VECTOR('',#1520,1.);
#526=VECTOR('',#1521,1.);
#527=VECTOR('',#1524,1.);
#528=VECTOR('',#1525,1.);
#529=VECTOR('',#1528,1.);
#530=VECTOR('',#1531,1.);
#531=VECTOR('',#1534,1.);
#532=VECTOR('',#1535,1.);
#533=VECTOR('',#1536,1.);
#534=VECTOR('',#1539,1.);
#535=VECTOR('',#1540,1.);
#536=VECTOR('',#1543,1.);
#537=VECTOR('',#1544,1.);
#538=VECTOR('',#1547,1.);
#539=VECTOR('',#1554,1.);
#540=VECTOR('',#1555,1.);
#541=VECTOR('',#1556,1.);
#542=VECTOR('',#1557,1.);
#543=VECTOR('',#1560,1.);
#544=VECTOR('',#1561,1.);
#545=VECTOR('',#1562,1.);
#546=VECTOR('',#1563,1.);
#547=VECTOR('',#1566,1.);
#548=VECTOR('',#1567,1.);
#549=VECTOR('',#1570,1.);
#550=VECTOR('',#1571,1.);
#551=VECTOR('',#1572,1.);
#552=VECTOR('',#1573,1.);
#553=VECTOR('',#1574,1.);
#554=VECTOR('',#1577,1.);
#555=VECTOR('',#1578,1.);
#556=VECTOR('',#1581,1.);
#557=VECTOR('',#1582,1.);
#558=VECTOR('',#1583,1.);
#559=VECTOR('',#1586,1.);
#560=VECTOR('',#1587,1.);
#561=VECTOR('',#1590,1.);
#562=VECTOR('',#1591,1.);
#563=VECTOR('',#1600,1.);
#564=VECTOR('',#1601,1.);
#565=VECTOR('',#1602,1.);
#566=VECTOR('',#1603,1.);
#567=VECTOR('',#1606,1.);
#568=VECTOR('',#1607,1.);
#569=VECTOR('',#1608,1.);
#570=VECTOR('',#1611,1.);
#571=VECTOR('',#1612,1.);
#572=VECTOR('',#1613,1.);
#573=VECTOR('',#1616,1.);
#574=VECTOR('',#1617,1.);
#575=VECTOR('',#1626,1.);
#576=VECTOR('',#1627,1.);
#577=VECTOR('',#1628,1.);
#578=VECTOR('',#1629,1.);
#579=VECTOR('',#1632,1.);
#580=VECTOR('',#1633,1.);
#581=VECTOR('',#1634,1.);
#582=VECTOR('',#1637,1.);
#583=VECTOR('',#1638,1.);
#584=VECTOR('',#1639,1.);
#585=VECTOR('',#1642,1.);
#586=VECTOR('',#1643,1.);
#587=VECTOR('',#1654,0.6);
#588=VECTOR('',#1663,0.6);
#589=VECTOR('',#1672,1.25);
#590=VECTOR('',#1685,0.4);
#591=CIRCLE('',#1269,0.409999999999997);
#592=CIRCLE('',#1270,0.409999999999997);
#593=CIRCLE('',#1273,0.409999999999997);
#594=CIRCLE('',#1274,0.409999999999997);
#595=CIRCLE('',#1277,0.409999999999997);
#596=CIRCLE('',#1278,0.409999999999997);
#597=CIRCLE('',#1281,0.409999999999997);
#598=CIRCLE('',#1282,0.409999999999997);
#599=CIRCLE('',#1285,0.620000000000001);
#600=CIRCLE('',#1286,0.620000000000001);
#601=CIRCLE('',#1289,0.620000000000005);
#602=CIRCLE('',#1290,0.620000000000005);
#603=CIRCLE('',#1341,0.6);
#604=CIRCLE('',#1342,0.6);
#605=CIRCLE('',#1345,0.6);
#606=CIRCLE('',#1346,0.6);
#607=CIRCLE('',#1349,1.25);
#608=CIRCLE('',#1350,1.25);
#609=CIRCLE('',#1355,0.4);
#610=CIRCLE('',#1356,0.4);
#611=VERTEX_POINT('',#1753);
#612=VERTEX_POINT('',#1755);
#613=VERTEX_POINT('',#1760);
#614=VERTEX_POINT('',#1762);
#615=VERTEX_POINT('',#1767);
#616=VERTEX_POINT('',#1769);
#617=VERTEX_POINT('',#1774);
#618=VERTEX_POINT('',#1776);
#619=VERTEX_POINT('',#1781);
#620=VERTEX_POINT('',#1783);
#621=VERTEX_POINT('',#1788);
#622=VERTEX_POINT('',#1790);
#623=VERTEX_POINT('',#1795);
#624=VERTEX_POINT('',#1796);
#625=VERTEX_POINT('',#1798);
#626=VERTEX_POINT('',#1800);
#627=VERTEX_POINT('',#1804);
#628=VERTEX_POINT('',#1805);
#629=VERTEX_POINT('',#1807);
#630=VERTEX_POINT('',#1809);
#631=VERTEX_POINT('',#1813);
#632=VERTEX_POINT('',#1814);
#633=VERTEX_POINT('',#1816);
#634=VERTEX_POINT('',#1818);
#635=VERTEX_POINT('',#1822);
#636=VERTEX_POINT('',#1823);
#637=VERTEX_POINT('',#1825);
#638=VERTEX_POINT('',#1827);
#639=VERTEX_POINT('',#1831);
#640=VERTEX_POINT('',#1833);
#641=VERTEX_POINT('',#1835);
#642=VERTEX_POINT('',#1837);
#643=VERTEX_POINT('',#1840);
#644=VERTEX_POINT('',#1842);
#645=VERTEX_POINT('',#1845);
#646=VERTEX_POINT('',#1847);
#647=VERTEX_POINT('',#1849);
#648=VERTEX_POINT('',#1851);
#649=VERTEX_POINT('',#1854);
#650=VERTEX_POINT('',#1856);
#651=VERTEX_POINT('',#1860);
#652=VERTEX_POINT('',#1864);
#653=VERTEX_POINT('',#1868);
#654=VERTEX_POINT('',#1872);
#655=VERTEX_POINT('',#1880);
#656=VERTEX_POINT('',#1884);
#657=VERTEX_POINT('',#1888);
#658=VERTEX_POINT('',#1892);
#659=VERTEX_POINT('',#1900);
#660=VERTEX_POINT('',#1902);
#661=VERTEX_POINT('',#1906);
#662=VERTEX_POINT('',#1910);
#663=VERTEX_POINT('',#1918);
#664=VERTEX_POINT('',#1919);
#665=VERTEX_POINT('',#1921);
#666=VERTEX_POINT('',#1923);
#667=VERTEX_POINT('',#1927);
#668=VERTEX_POINT('',#1928);
#669=VERTEX_POINT('',#1930);
#670=VERTEX_POINT('',#1932);
#671=VERTEX_POINT('',#1939);
#672=VERTEX_POINT('',#1941);
#673=VERTEX_POINT('',#1943);
#674=VERTEX_POINT('',#1945);
#675=VERTEX_POINT('',#1949);
#676=VERTEX_POINT('',#1953);
#677=VERTEX_POINT('',#1955);
#678=VERTEX_POINT('',#1959);
#679=VERTEX_POINT('',#1969);
#680=VERTEX_POINT('',#1970);
#681=VERTEX_POINT('',#1972);
#682=VERTEX_POINT('',#1974);
#683=VERTEX_POINT('',#1978);
#684=VERTEX_POINT('',#1980);
#685=VERTEX_POINT('',#1984);
#686=VERTEX_POINT('',#1986);
#687=VERTEX_POINT('',#1996);
#688=VERTEX_POINT('',#1997);
#689=VERTEX_POINT('',#1999);
#690=VERTEX_POINT('',#2001);
#691=VERTEX_POINT('',#2005);
#692=VERTEX_POINT('',#2007);
#693=VERTEX_POINT('',#2011);
#694=VERTEX_POINT('',#2013);
#695=VERTEX_POINT('',#2023);
#696=VERTEX_POINT('',#2025);
#697=VERTEX_POINT('',#2030);
#698=VERTEX_POINT('',#2032);
#699=VERTEX_POINT('',#2037);
#700=VERTEX_POINT('',#2039);
#701=VERTEX_POINT('',#2046);
#702=VERTEX_POINT('',#2048);
#703=EDGE_CURVE('',#611,#611,#591,.T.);
#704=EDGE_CURVE('',#611,#612,#355,.T.);
#705=EDGE_CURVE('',#612,#612,#592,.T.);
#706=EDGE_CURVE('',#613,#613,#593,.T.);
#707=EDGE_CURVE('',#613,#614,#356,.T.);
#708=EDGE_CURVE('',#614,#614,#594,.T.);
#709=EDGE_CURVE('',#615,#615,#595,.T.);
#710=EDGE_CURVE('',#615,#616,#357,.T.);
#711=EDGE_CURVE('',#616,#616,#596,.T.);
#712=EDGE_CURVE('',#617,#617,#597,.T.);
#713=EDGE_CURVE('',#617,#618,#358,.T.);
#714=EDGE_CURVE('',#618,#618,#598,.T.);
#715=EDGE_CURVE('',#619,#619,#599,.T.);
#716=EDGE_CURVE('',#619,#620,#359,.T.);
#717=EDGE_CURVE('',#620,#620,#600,.T.);
#718=EDGE_CURVE('',#621,#621,#601,.T.);
#719=EDGE_CURVE('',#621,#622,#360,.T.);
#720=EDGE_CURVE('',#622,#622,#602,.T.);
#721=EDGE_CURVE('',#623,#624,#361,.T.);
#722=EDGE_CURVE('',#625,#623,#362,.T.);
#723=EDGE_CURVE('',#626,#625,#363,.T.);
#724=EDGE_CURVE('',#624,#626,#364,.T.);
#725=EDGE_CURVE('',#627,#628,#365,.T.);
#726=EDGE_CURVE('',#629,#627,#366,.T.);
#727=EDGE_CURVE('',#630,#629,#367,.T.);
#728=EDGE_CURVE('',#628,#630,#368,.T.);
#729=EDGE_CURVE('',#631,#632,#369,.T.);
#730=EDGE_CURVE('',#633,#631,#370,.T.);
#731=EDGE_CURVE('',#634,#633,#371,.T.);
#732=EDGE_CURVE('',#634,#632,#372,.T.);
#733=EDGE_CURVE('',#635,#636,#373,.T.);
#734=EDGE_CURVE('',#637,#635,#374,.T.);
#735=EDGE_CURVE('',#638,#637,#375,.T.);
#736=EDGE_CURVE('',#638,#636,#376,.T.);
#737=EDGE_CURVE('',#639,#627,#377,.T.);
#738=EDGE_CURVE('',#640,#639,#378,.T.);
#739=EDGE_CURVE('',#641,#640,#379,.T.);
#740=EDGE_CURVE('',#642,#641,#380,.T.);
#741=EDGE_CURVE('',#636,#642,#381,.T.);
#742=EDGE_CURVE('',#638,#643,#382,.T.);
#743=EDGE_CURVE('',#644,#643,#383,.T.);
#744=EDGE_CURVE('',#632,#644,#384,.T.);
#745=EDGE_CURVE('',#634,#645,#385,.T.);
#746=EDGE_CURVE('',#646,#645,#386,.T.);
#747=EDGE_CURVE('',#647,#646,#387,.T.);
#748=EDGE_CURVE('',#648,#647,#388,.T.);
#749=EDGE_CURVE('',#648,#625,#389,.T.);
#750=EDGE_CURVE('',#649,#623,#390,.T.);
#751=EDGE_CURVE('',#650,#649,#391,.T.);
#752=EDGE_CURVE('',#650,#629,#392,.T.);
#753=EDGE_CURVE('',#651,#642,#393,.T.);
#754=EDGE_CURVE('',#635,#651,#394,.T.);
#755=EDGE_CURVE('',#652,#628,#395,.T.);
#756=EDGE_CURVE('',#639,#652,#396,.T.);
#757=EDGE_CURVE('',#653,#651,#397,.T.);
#758=EDGE_CURVE('',#653,#637,#398,.T.);
#759=EDGE_CURVE('',#630,#654,#399,.T.);
#760=EDGE_CURVE('',#654,#652,#400,.T.);
#761=EDGE_CURVE('',#643,#653,#401,.T.);
#762=EDGE_CURVE('',#654,#650,#402,.T.);
#763=EDGE_CURVE('',#655,#644,#403,.T.);
#764=EDGE_CURVE('',#631,#655,#404,.T.);
#765=EDGE_CURVE('',#656,#624,#405,.T.);
#766=EDGE_CURVE('',#649,#656,#406,.T.);
#767=EDGE_CURVE('',#657,#655,#407,.T.);
#768=EDGE_CURVE('',#657,#633,#408,.T.);
#769=EDGE_CURVE('',#626,#658,#409,.T.);
#770=EDGE_CURVE('',#658,#656,#410,.T.);
#771=EDGE_CURVE('',#645,#657,#411,.T.);
#772=EDGE_CURVE('',#658,#648,#412,.T.);
#773=EDGE_CURVE('',#647,#659,#413,.T.);
#774=EDGE_CURVE('',#659,#660,#414,.T.);
#775=EDGE_CURVE('',#640,#660,#415,.T.);
#776=EDGE_CURVE('',#661,#646,#416,.T.);
#777=EDGE_CURVE('',#659,#661,#417,.T.);
#778=EDGE_CURVE('',#662,#641,#418,.T.);
#779=EDGE_CURVE('',#661,#662,#419,.T.);
#780=EDGE_CURVE('',#660,#662,#420,.T.);
#781=EDGE_CURVE('',#663,#664,#421,.T.);
#782=EDGE_CURVE('',#665,#663,#422,.T.);
#783=EDGE_CURVE('',#666,#665,#423,.T.);
#784=EDGE_CURVE('',#664,#666,#424,.T.);
#785=EDGE_CURVE('',#667,#668,#425,.T.);
#786=EDGE_CURVE('',#669,#667,#426,.T.);
#787=EDGE_CURVE('',#670,#669,#427,.T.);
#788=EDGE_CURVE('',#668,#670,#428,.T.);
#789=EDGE_CURVE('',#666,#669,#429,.T.);
#790=EDGE_CURVE('',#670,#665,#430,.T.);
#791=EDGE_CURVE('',#671,#663,#431,.T.);
#792=EDGE_CURVE('',#672,#671,#432,.T.);
#793=EDGE_CURVE('',#672,#673,#433,.T.);
#794=EDGE_CURVE('',#673,#674,#434,.T.);
#795=EDGE_CURVE('',#668,#674,#435,.T.);
#796=EDGE_CURVE('',#664,#675,#436,.T.);
#797=EDGE_CURVE('',#675,#671,#437,.T.);
#798=EDGE_CURVE('',#673,#676,#438,.T.);
#799=EDGE_CURVE('',#676,#677,#439,.T.);
#800=EDGE_CURVE('',#674,#677,#440,.T.);
#801=EDGE_CURVE('',#678,#672,#441,.T.);
#802=EDGE_CURVE('',#678,#675,#442,.T.);
#803=EDGE_CURVE('',#677,#667,#443,.T.);
#804=EDGE_CURVE('',#676,#678,#444,.T.);
#805=EDGE_CURVE('',#679,#680,#445,.T.);
#806=EDGE_CURVE('',#680,#681,#446,.T.);
#807=EDGE_CURVE('',#682,#681,#447,.T.);
#808=EDGE_CURVE('',#679,#682,#448,.T.);
#809=EDGE_CURVE('',#683,#679,#449,.T.);
#810=EDGE_CURVE('',#684,#682,#450,.T.);
#811=EDGE_CURVE('',#683,#684,#451,.T.);
#812=EDGE_CURVE('',#685,#683,#452,.T.);
#813=EDGE_CURVE('',#686,#684,#453,.T.);
#814=EDGE_CURVE('',#685,#686,#454,.T.);
#815=EDGE_CURVE('',#680,#685,#455,.T.);
#816=EDGE_CURVE('',#681,#686,#456,.T.);
#817=EDGE_CURVE('',#687,#688,#457,.T.);
#818=EDGE_CURVE('',#688,#689,#458,.T.);
#819=EDGE_CURVE('',#690,#689,#459,.T.);
#820=EDGE_CURVE('',#687,#690,#460,.T.);
#821=EDGE_CURVE('',#691,#687,#461,.T.);
#822=EDGE_CURVE('',#692,#690,#462,.T.);
#823=EDGE_CURVE('',#691,#692,#463,.T.);
#824=EDGE_CURVE('',#693,#691,#464,.T.);
#825=EDGE_CURVE('',#694,#692,#465,.T.);
#826=EDGE_CURVE('',#693,#694,#466,.T.);
#827=EDGE_CURVE('',#688,#693,#467,.T.);
#828=EDGE_CURVE('',#689,#694,#468,.T.);
#829=EDGE_CURVE('',#695,#695,#603,.T.);
#830=EDGE_CURVE('',#695,#696,#469,.T.);
#831=EDGE_CURVE('',#696,#696,#604,.T.);
#832=EDGE_CURVE('',#697,#697,#605,.T.);
#833=EDGE_CURVE('',#697,#698,#470,.T.);
#834=EDGE_CURVE('',#698,#698,#606,.T.);
#835=EDGE_CURVE('',#699,#699,#607,.T.);
#836=EDGE_CURVE('',#699,#700,#471,.T.);
#837=EDGE_CURVE('',#700,#700,#608,.T.);
#838=EDGE_CURVE('',#701,#701,#609,.T.);
#839=EDGE_CURVE('',#701,#702,#472,.T.);
#840=EDGE_CURVE('',#702,#702,#610,.T.);
#841=ORIENTED_EDGE('',*,*,#703,.F.);
#842=ORIENTED_EDGE('',*,*,#704,.T.);
#843=ORIENTED_EDGE('',*,*,#705,.T.);
#844=ORIENTED_EDGE('',*,*,#704,.F.);
#845=ORIENTED_EDGE('',*,*,#705,.F.);
#846=ORIENTED_EDGE('',*,*,#706,.F.);
#847=ORIENTED_EDGE('',*,*,#707,.T.);
#848=ORIENTED_EDGE('',*,*,#708,.T.);
#849=ORIENTED_EDGE('',*,*,#707,.F.);
#850=ORIENTED_EDGE('',*,*,#708,.F.);
#851=ORIENTED_EDGE('',*,*,#709,.F.);
#852=ORIENTED_EDGE('',*,*,#710,.T.);
#853=ORIENTED_EDGE('',*,*,#711,.T.);
#854=ORIENTED_EDGE('',*,*,#710,.F.);
#855=ORIENTED_EDGE('',*,*,#711,.F.);
#856=ORIENTED_EDGE('',*,*,#712,.F.);
#857=ORIENTED_EDGE('',*,*,#713,.T.);
#858=ORIENTED_EDGE('',*,*,#714,.T.);
#859=ORIENTED_EDGE('',*,*,#713,.F.);
#860=ORIENTED_EDGE('',*,*,#714,.F.);
#861=ORIENTED_EDGE('',*,*,#715,.F.);
#862=ORIENTED_EDGE('',*,*,#716,.T.);
#863=ORIENTED_EDGE('',*,*,#717,.T.);
#864=ORIENTED_EDGE('',*,*,#716,.F.);
#865=ORIENTED_EDGE('',*,*,#717,.F.);
#866=ORIENTED_EDGE('',*,*,#718,.F.);
#867=ORIENTED_EDGE('',*,*,#719,.T.);
#868=ORIENTED_EDGE('',*,*,#720,.T.);
#869=ORIENTED_EDGE('',*,*,#719,.F.);
#870=ORIENTED_EDGE('',*,*,#720,.F.);
#871=ORIENTED_EDGE('',*,*,#721,.F.);
#872=ORIENTED_EDGE('',*,*,#722,.F.);
#873=ORIENTED_EDGE('',*,*,#723,.F.);
#874=ORIENTED_EDGE('',*,*,#724,.F.);
#875=ORIENTED_EDGE('',*,*,#725,.F.);
#876=ORIENTED_EDGE('',*,*,#726,.F.);
#877=ORIENTED_EDGE('',*,*,#727,.F.);
#878=ORIENTED_EDGE('',*,*,#728,.F.);
#879=ORIENTED_EDGE('',*,*,#729,.F.);
#880=ORIENTED_EDGE('',*,*,#730,.F.);
#881=ORIENTED_EDGE('',*,*,#731,.F.);
#882=ORIENTED_EDGE('',*,*,#732,.T.);
#883=ORIENTED_EDGE('',*,*,#733,.F.);
#884=ORIENTED_EDGE('',*,*,#734,.F.);
#885=ORIENTED_EDGE('',*,*,#735,.F.);
#886=ORIENTED_EDGE('',*,*,#736,.T.);
#887=ORIENTED_EDGE('',*,*,#737,.F.);
#888=ORIENTED_EDGE('',*,*,#738,.F.);
#889=ORIENTED_EDGE('',*,*,#739,.F.);
#890=ORIENTED_EDGE('',*,*,#740,.F.);
#891=ORIENTED_EDGE('',*,*,#741,.F.);
#892=ORIENTED_EDGE('',*,*,#736,.F.);
#893=ORIENTED_EDGE('',*,*,#742,.T.);
#894=ORIENTED_EDGE('',*,*,#743,.F.);
#895=ORIENTED_EDGE('',*,*,#744,.F.);
#896=ORIENTED_EDGE('',*,*,#732,.F.);
#897=ORIENTED_EDGE('',*,*,#745,.T.);
#898=ORIENTED_EDGE('',*,*,#746,.F.);
#899=ORIENTED_EDGE('',*,*,#747,.F.);
#900=ORIENTED_EDGE('',*,*,#748,.F.);
#901=ORIENTED_EDGE('',*,*,#749,.T.);
#902=ORIENTED_EDGE('',*,*,#722,.T.);
#903=ORIENTED_EDGE('',*,*,#750,.F.);
#904=ORIENTED_EDGE('',*,*,#751,.F.);
#905=ORIENTED_EDGE('',*,*,#752,.T.);
#906=ORIENTED_EDGE('',*,*,#726,.T.);
#907=ORIENTED_EDGE('',*,*,#733,.T.);
#908=ORIENTED_EDGE('',*,*,#741,.T.);
#909=ORIENTED_EDGE('',*,*,#753,.F.);
#910=ORIENTED_EDGE('',*,*,#754,.F.);
#911=ORIENTED_EDGE('',*,*,#725,.T.);
#912=ORIENTED_EDGE('',*,*,#755,.F.);
#913=ORIENTED_EDGE('',*,*,#756,.F.);
#914=ORIENTED_EDGE('',*,*,#737,.T.);
#915=ORIENTED_EDGE('',*,*,#734,.T.);
#916=ORIENTED_EDGE('',*,*,#754,.T.);
#917=ORIENTED_EDGE('',*,*,#757,.F.);
#918=ORIENTED_EDGE('',*,*,#758,.T.);
#919=ORIENTED_EDGE('',*,*,#718,.T.);
#920=ORIENTED_EDGE('',*,*,#728,.T.);
#921=ORIENTED_EDGE('',*,*,#759,.T.);
#922=ORIENTED_EDGE('',*,*,#760,.T.);
#923=ORIENTED_EDGE('',*,*,#755,.T.);
#924=ORIENTED_EDGE('',*,*,#735,.T.);
#925=ORIENTED_EDGE('',*,*,#758,.F.);
#926=ORIENTED_EDGE('',*,*,#761,.F.);
#927=ORIENTED_EDGE('',*,*,#742,.F.);
#928=ORIENTED_EDGE('',*,*,#727,.T.);
#929=ORIENTED_EDGE('',*,*,#752,.F.);
#930=ORIENTED_EDGE('',*,*,#762,.F.);
#931=ORIENTED_EDGE('',*,*,#759,.F.);
#932=ORIENTED_EDGE('',*,*,#729,.T.);
#933=ORIENTED_EDGE('',*,*,#744,.T.);
#934=ORIENTED_EDGE('',*,*,#763,.F.);
#935=ORIENTED_EDGE('',*,*,#764,.F.);
#936=ORIENTED_EDGE('',*,*,#721,.T.);
#937=ORIENTED_EDGE('',*,*,#765,.F.);
#938=ORIENTED_EDGE('',*,*,#766,.F.);
#939=ORIENTED_EDGE('',*,*,#750,.T.);
#940=ORIENTED_EDGE('',*,*,#730,.T.);
#941=ORIENTED_EDGE('',*,*,#764,.T.);
#942=ORIENTED_EDGE('',*,*,#767,.F.);
#943=ORIENTED_EDGE('',*,*,#768,.T.);
#944=ORIENTED_EDGE('',*,*,#715,.T.);
#945=ORIENTED_EDGE('',*,*,#724,.T.);
#946=ORIENTED_EDGE('',*,*,#769,.T.);
#947=ORIENTED_EDGE('',*,*,#770,.T.);
#948=ORIENTED_EDGE('',*,*,#765,.T.);
#949=ORIENTED_EDGE('',*,*,#731,.T.);
#950=ORIENTED_EDGE('',*,*,#768,.F.);
#951=ORIENTED_EDGE('',*,*,#771,.F.);
#952=ORIENTED_EDGE('',*,*,#745,.F.);
#953=ORIENTED_EDGE('',*,*,#723,.T.);
#954=ORIENTED_EDGE('',*,*,#749,.F.);
#955=ORIENTED_EDGE('',*,*,#772,.F.);
#956=ORIENTED_EDGE('',*,*,#769,.F.);
#957=ORIENTED_EDGE('',*,*,#762,.T.);
#958=ORIENTED_EDGE('',*,*,#751,.T.);
#959=ORIENTED_EDGE('',*,*,#766,.T.);
#960=ORIENTED_EDGE('',*,*,#770,.F.);
#961=ORIENTED_EDGE('',*,*,#772,.T.);
#962=ORIENTED_EDGE('',*,*,#748,.T.);
#963=ORIENTED_EDGE('',*,*,#773,.T.);
#964=ORIENTED_EDGE('',*,*,#774,.T.);
#965=ORIENTED_EDGE('',*,*,#775,.F.);
#966=ORIENTED_EDGE('',*,*,#738,.T.);
#967=ORIENTED_EDGE('',*,*,#756,.T.);
#968=ORIENTED_EDGE('',*,*,#760,.F.);
#969=ORIENTED_EDGE('',*,*,#747,.T.);
#970=ORIENTED_EDGE('',*,*,#776,.F.);
#971=ORIENTED_EDGE('',*,*,#777,.F.);
#972=ORIENTED_EDGE('',*,*,#773,.F.);
#973=ORIENTED_EDGE('',*,*,#761,.T.);
#974=ORIENTED_EDGE('',*,*,#757,.T.);
#975=ORIENTED_EDGE('',*,*,#753,.T.);
#976=ORIENTED_EDGE('',*,*,#740,.T.);
#977=ORIENTED_EDGE('',*,*,#778,.F.);
#978=ORIENTED_EDGE('',*,*,#779,.F.);
#979=ORIENTED_EDGE('',*,*,#776,.T.);
#980=ORIENTED_EDGE('',*,*,#746,.T.);
#981=ORIENTED_EDGE('',*,*,#771,.T.);
#982=ORIENTED_EDGE('',*,*,#767,.T.);
#983=ORIENTED_EDGE('',*,*,#763,.T.);
#984=ORIENTED_EDGE('',*,*,#743,.T.);
#985=ORIENTED_EDGE('',*,*,#777,.T.);
#986=ORIENTED_EDGE('',*,*,#779,.T.);
#987=ORIENTED_EDGE('',*,*,#780,.F.);
#988=ORIENTED_EDGE('',*,*,#774,.F.);
#989=ORIENTED_EDGE('',*,*,#703,.T.);
#990=ORIENTED_EDGE('',*,*,#706,.T.);
#991=ORIENTED_EDGE('',*,*,#709,.T.);
#992=ORIENTED_EDGE('',*,*,#712,.T.);
#993=ORIENTED_EDGE('',*,*,#739,.T.);
#994=ORIENTED_EDGE('',*,*,#775,.T.);
#995=ORIENTED_EDGE('',*,*,#780,.T.);
#996=ORIENTED_EDGE('',*,*,#778,.T.);
#997=ORIENTED_EDGE('',*,*,#781,.F.);
#998=ORIENTED_EDGE('',*,*,#782,.F.);
#999=ORIENTED_EDGE('',*,*,#783,.F.);
#1000=ORIENTED_EDGE('',*,*,#784,.F.);
#1001=ORIENTED_EDGE('',*,*,#785,.F.);
#1002=ORIENTED_EDGE('',*,*,#786,.F.);
#1003=ORIENTED_EDGE('',*,*,#787,.F.);
#1004=ORIENTED_EDGE('',*,*,#788,.F.);
#1005=ORIENTED_EDGE('',*,*,#789,.F.);
#1006=ORIENTED_EDGE('',*,*,#783,.T.);
#1007=ORIENTED_EDGE('',*,*,#790,.F.);
#1008=ORIENTED_EDGE('',*,*,#787,.T.);
#1009=ORIENTED_EDGE('',*,*,#788,.T.);
#1010=ORIENTED_EDGE('',*,*,#790,.T.);
#1011=ORIENTED_EDGE('',*,*,#782,.T.);
#1012=ORIENTED_EDGE('',*,*,#791,.F.);
#1013=ORIENTED_EDGE('',*,*,#792,.F.);
#1014=ORIENTED_EDGE('',*,*,#793,.T.);
#1015=ORIENTED_EDGE('',*,*,#794,.T.);
#1016=ORIENTED_EDGE('',*,*,#795,.F.);
#1017=ORIENTED_EDGE('',*,*,#781,.T.);
#1018=ORIENTED_EDGE('',*,*,#796,.T.);
#1019=ORIENTED_EDGE('',*,*,#797,.T.);
#1020=ORIENTED_EDGE('',*,*,#791,.T.);
#1021=ORIENTED_EDGE('',*,*,#798,.T.);
#1022=ORIENTED_EDGE('',*,*,#799,.T.);
#1023=ORIENTED_EDGE('',*,*,#800,.F.);
#1024=ORIENTED_EDGE('',*,*,#794,.F.);
#1025=ORIENTED_EDGE('',*,*,#801,.T.);
#1026=ORIENTED_EDGE('',*,*,#792,.T.);
#1027=ORIENTED_EDGE('',*,*,#797,.F.);
#1028=ORIENTED_EDGE('',*,*,#802,.F.);
#1029=ORIENTED_EDGE('',*,*,#786,.T.);
#1030=ORIENTED_EDGE('',*,*,#803,.F.);
#1031=ORIENTED_EDGE('',*,*,#799,.F.);
#1032=ORIENTED_EDGE('',*,*,#804,.T.);
#1033=ORIENTED_EDGE('',*,*,#802,.T.);
#1034=ORIENTED_EDGE('',*,*,#796,.F.);
#1035=ORIENTED_EDGE('',*,*,#784,.T.);
#1036=ORIENTED_EDGE('',*,*,#789,.T.);
#1037=ORIENTED_EDGE('',*,*,#785,.T.);
#1038=ORIENTED_EDGE('',*,*,#795,.T.);
#1039=ORIENTED_EDGE('',*,*,#800,.T.);
#1040=ORIENTED_EDGE('',*,*,#803,.T.);
#1041=ORIENTED_EDGE('',*,*,#804,.F.);
#1042=ORIENTED_EDGE('',*,*,#798,.F.);
#1043=ORIENTED_EDGE('',*,*,#793,.F.);
#1044=ORIENTED_EDGE('',*,*,#801,.F.);
#1045=ORIENTED_EDGE('',*,*,#805,.T.);
#1046=ORIENTED_EDGE('',*,*,#806,.T.);
#1047=ORIENTED_EDGE('',*,*,#807,.F.);
#1048=ORIENTED_EDGE('',*,*,#808,.F.);
#1049=ORIENTED_EDGE('',*,*,#809,.T.);
#1050=ORIENTED_EDGE('',*,*,#808,.T.);
#1051=ORIENTED_EDGE('',*,*,#810,.F.);
#1052=ORIENTED_EDGE('',*,*,#811,.F.);
#1053=ORIENTED_EDGE('',*,*,#812,.T.);
#1054=ORIENTED_EDGE('',*,*,#811,.T.);
#1055=ORIENTED_EDGE('',*,*,#813,.F.);
#1056=ORIENTED_EDGE('',*,*,#814,.F.);
#1057=ORIENTED_EDGE('',*,*,#815,.T.);
#1058=ORIENTED_EDGE('',*,*,#814,.T.);
#1059=ORIENTED_EDGE('',*,*,#816,.F.);
#1060=ORIENTED_EDGE('',*,*,#806,.F.);
#1061=ORIENTED_EDGE('',*,*,#816,.T.);
#1062=ORIENTED_EDGE('',*,*,#813,.T.);
#1063=ORIENTED_EDGE('',*,*,#810,.T.);
#1064=ORIENTED_EDGE('',*,*,#807,.T.);
#1065=ORIENTED_EDGE('',*,*,#815,.F.);
#1066=ORIENTED_EDGE('',*,*,#805,.F.);
#1067=ORIENTED_EDGE('',*,*,#809,.F.);
#1068=ORIENTED_EDGE('',*,*,#812,.F.);
#1069=ORIENTED_EDGE('',*,*,#817,.T.);
#1070=ORIENTED_EDGE('',*,*,#818,.T.);
#1071=ORIENTED_EDGE('',*,*,#819,.F.);
#1072=ORIENTED_EDGE('',*,*,#820,.F.);
#1073=ORIENTED_EDGE('',*,*,#821,.T.);
#1074=ORIENTED_EDGE('',*,*,#820,.T.);
#1075=ORIENTED_EDGE('',*,*,#822,.F.);
#1076=ORIENTED_EDGE('',*,*,#823,.F.);
#1077=ORIENTED_EDGE('',*,*,#824,.T.);
#1078=ORIENTED_EDGE('',*,*,#823,.T.);
#1079=ORIENTED_EDGE('',*,*,#825,.F.);
#1080=ORIENTED_EDGE('',*,*,#826,.F.);
#1081=ORIENTED_EDGE('',*,*,#827,.T.);
#1082=ORIENTED_EDGE('',*,*,#826,.T.);
#1083=ORIENTED_EDGE('',*,*,#828,.F.);
#1084=ORIENTED_EDGE('',*,*,#818,.F.);
#1085=ORIENTED_EDGE('',*,*,#828,.T.);
#1086=ORIENTED_EDGE('',*,*,#825,.T.);
#1087=ORIENTED_EDGE('',*,*,#822,.T.);
#1088=ORIENTED_EDGE('',*,*,#819,.T.);
#1089=ORIENTED_EDGE('',*,*,#827,.F.);
#1090=ORIENTED_EDGE('',*,*,#817,.F.);
#1091=ORIENTED_EDGE('',*,*,#821,.F.);
#1092=ORIENTED_EDGE('',*,*,#824,.F.);
#1093=ORIENTED_EDGE('',*,*,#829,.F.);
#1094=ORIENTED_EDGE('',*,*,#830,.T.);
#1095=ORIENTED_EDGE('',*,*,#831,.F.);
#1096=ORIENTED_EDGE('',*,*,#830,.F.);
#1097=ORIENTED_EDGE('',*,*,#829,.T.);
#1098=ORIENTED_EDGE('',*,*,#832,.F.);
#1099=ORIENTED_EDGE('',*,*,#833,.T.);
#1100=ORIENTED_EDGE('',*,*,#834,.T.);
#1101=ORIENTED_EDGE('',*,*,#833,.F.);
#1102=ORIENTED_EDGE('',*,*,#834,.F.);
#1103=ORIENTED_EDGE('',*,*,#835,.F.);
#1104=ORIENTED_EDGE('',*,*,#836,.T.);
#1105=ORIENTED_EDGE('',*,*,#837,.T.);
#1106=ORIENTED_EDGE('',*,*,#836,.F.);
#1107=ORIENTED_EDGE('',*,*,#835,.T.);
#1108=ORIENTED_EDGE('',*,*,#831,.T.);
#1109=ORIENTED_EDGE('',*,*,#837,.F.);
#1110=ORIENTED_EDGE('',*,*,#832,.T.);
#1111=ORIENTED_EDGE('',*,*,#838,.F.);
#1112=ORIENTED_EDGE('',*,*,#839,.T.);
#1113=ORIENTED_EDGE('',*,*,#840,.T.);
#1114=ORIENTED_EDGE('',*,*,#839,.F.);
#1115=ORIENTED_EDGE('',*,*,#838,.T.);
#1116=ORIENTED_EDGE('',*,*,#840,.F.);
#1117=CYLINDRICAL_SURFACE('',#1268,0.409999999999997);
#1118=CYLINDRICAL_SURFACE('',#1272,0.409999999999997);
#1119=CYLINDRICAL_SURFACE('',#1276,0.409999999999997);
#1120=CYLINDRICAL_SURFACE('',#1280,0.409999999999997);
#1121=CYLINDRICAL_SURFACE('',#1284,0.620000000000001);
#1122=CYLINDRICAL_SURFACE('',#1288,0.620000000000005);
#1123=CYLINDRICAL_SURFACE('',#1340,0.6);
#1124=CYLINDRICAL_SURFACE('',#1344,0.6);
#1125=CYLINDRICAL_SURFACE('',#1348,1.25);
#1126=CYLINDRICAL_SURFACE('',#1354,0.4);
#1127=ADVANCED_FACE('',(#215),#1117,.F.);
#1128=ADVANCED_FACE('',(#216),#159,.F.);
#1129=ADVANCED_FACE('',(#217),#1118,.F.);
#1130=ADVANCED_FACE('',(#218),#160,.F.);
#1131=ADVANCED_FACE('',(#219),#1119,.F.);
#1132=ADVANCED_FACE('',(#220),#161,.F.);
#1133=ADVANCED_FACE('',(#221),#1120,.F.);
#1134=ADVANCED_FACE('',(#222),#162,.F.);
#1135=ADVANCED_FACE('',(#223),#1121,.F.);
#1136=ADVANCED_FACE('',(#224),#163,.T.);
#1137=ADVANCED_FACE('',(#225),#1122,.F.);
#1138=ADVANCED_FACE('',(#226),#164,.T.);
#1139=ADVANCED_FACE('',(#227),#165,.F.);
#1140=ADVANCED_FACE('',(#228),#166,.F.);
#1141=ADVANCED_FACE('',(#229),#167,.F.);
#1142=ADVANCED_FACE('',(#230),#168,.F.);
#1143=ADVANCED_FACE('',(#231),#169,.F.);
#1144=ADVANCED_FACE('',(#232),#170,.T.);
#1145=ADVANCED_FACE('',(#233),#171,.T.);
#1146=ADVANCED_FACE('',(#234,#151),#172,.T.);
#1147=ADVANCED_FACE('',(#235),#173,.T.);
#1148=ADVANCED_FACE('',(#236),#174,.F.);
#1149=ADVANCED_FACE('',(#237),#175,.F.);
#1150=ADVANCED_FACE('',(#238),#176,.T.);
#1151=ADVANCED_FACE('',(#239),#177,.T.);
#1152=ADVANCED_FACE('',(#240,#152),#178,.T.);
#1153=ADVANCED_FACE('',(#241),#179,.T.);
#1154=ADVANCED_FACE('',(#242),#180,.F.);
#1155=ADVANCED_FACE('',(#243),#181,.F.);
#1156=ADVANCED_FACE('',(#244),#182,.T.);
#1157=ADVANCED_FACE('',(#245),#183,.F.);
#1158=ADVANCED_FACE('',(#246),#184,.T.);
#1159=ADVANCED_FACE('',(#247,#153,#154,#155,#156),#185,.T.);
#1160=ADVANCED_FACE('',(#248),#186,.T.);
#1161=ADVANCED_FACE('',(#249),#187,.F.);
#1162=ADVANCED_FACE('',(#250),#188,.F.);
#1163=ADVANCED_FACE('',(#251),#189,.T.);
#1164=ADVANCED_FACE('',(#252),#190,.T.);
#1165=ADVANCED_FACE('',(#253),#191,.T.);
#1166=ADVANCED_FACE('',(#254),#192,.T.);
#1167=ADVANCED_FACE('',(#255),#193,.T.);
#1168=ADVANCED_FACE('',(#256),#194,.T.);
#1169=ADVANCED_FACE('',(#257),#195,.T.);
#1170=ADVANCED_FACE('',(#258),#196,.F.);
#1171=ADVANCED_FACE('',(#259),#197,.T.);
#1172=ADVANCED_FACE('',(#260),#198,.T.);
#1173=ADVANCED_FACE('',(#261),#199,.T.);
#1174=ADVANCED_FACE('',(#262),#200,.T.);
#1175=ADVANCED_FACE('',(#263),#201,.T.);
#1176=ADVANCED_FACE('',(#264),#202,.F.);
#1177=ADVANCED_FACE('',(#265),#203,.T.);
#1178=ADVANCED_FACE('',(#266),#204,.T.);
#1179=ADVANCED_FACE('',(#267),#205,.T.);
#1180=ADVANCED_FACE('',(#268),#206,.T.);
#1181=ADVANCED_FACE('',(#269),#207,.T.);
#1182=ADVANCED_FACE('',(#270),#208,.F.);
#1183=ADVANCED_FACE('',(#271),#1123,.T.);
#1184=ADVANCED_FACE('',(#272),#209,.T.);
#1185=ADVANCED_FACE('',(#273),#1124,.T.);
#1186=ADVANCED_FACE('',(#274),#210,.F.);
#1187=ADVANCED_FACE('',(#275),#1125,.T.);
#1188=ADVANCED_FACE('',(#276,#157),#211,.T.);
#1189=ADVANCED_FACE('',(#277,#158),#212,.F.);
#1190=ADVANCED_FACE('',(#278),#1126,.T.);
#1191=ADVANCED_FACE('',(#279),#213,.T.);
#1192=ADVANCED_FACE('',(#280),#214,.F.);
#1193=CLOSED_SHELL('',(#1127,#1128,#1129,#1130,#1131,#1132,#1133,#1134,
#1135,#1136,#1137,#1138,#1139,#1140,#1141,#1142,#1143,#1144,#1145,#1146,
#1147,#1148,#1149,#1150,#1151,#1152,#1153,#1154,#1155,#1156,#1157,#1158,
#1159,#1160));
#1194=CLOSED_SHELL('',(#1161,#1162,#1163,#1164,#1165,#1166,#1167,#1168,
#1169,#1170));
#1195=CLOSED_SHELL('',(#1171,#1172,#1173,#1174,#1175,#1176));
#1196=CLOSED_SHELL('',(#1177,#1178,#1179,#1180,#1181,#1182));
#1197=CLOSED_SHELL('',(#1183,#1184,#1185,#1186,#1187,#1188,#1189));
#1198=CLOSED_SHELL('',(#1190,#1191,#1192));
#1199=DERIVED_UNIT_ELEMENT(#1211,1.);
#1200=DERIVED_UNIT_ELEMENT(#2099,-3.);
#1201=DERIVED_UNIT_ELEMENT(#1211,1.);
#1202=DERIVED_UNIT_ELEMENT(#2099,-3.);
#1203=DERIVED_UNIT_ELEMENT(#1211,1.);
#1204=DERIVED_UNIT_ELEMENT(#2099,-3.);
#1205=DERIVED_UNIT_ELEMENT(#1211,1.);
#1206=DERIVED_UNIT_ELEMENT(#2099,-3.);
#1207=DERIVED_UNIT_ELEMENT(#1211,1.);
#1208=DERIVED_UNIT_ELEMENT(#2099,-3.);
#1209=DERIVED_UNIT_ELEMENT(#1211,1.);
#1210=DERIVED_UNIT_ELEMENT(#2099,-3.);
#1211=(
MASS_UNIT()
NAMED_UNIT(*)
SI_UNIT(.KILO.,.GRAM.)
);
#1212=DERIVED_UNIT((#1199,#1200));
#1213=DERIVED_UNIT((#1201,#1202));
#1214=DERIVED_UNIT((#1203,#1204));
#1215=DERIVED_UNIT((#1205,#1206));
#1216=DERIVED_UNIT((#1207,#1208));
#1217=DERIVED_UNIT((#1209,#1210));
#1218=MEASURE_REPRESENTATION_ITEM('density measure',
POSITIVE_RATIO_MEASURE(7850.),#1212);
#1219=MEASURE_REPRESENTATION_ITEM('density measure',
POSITIVE_RATIO_MEASURE(7850.),#1213);
#1220=MEASURE_REPRESENTATION_ITEM('density measure',
POSITIVE_RATIO_MEASURE(7850.),#1214);
#1221=MEASURE_REPRESENTATION_ITEM('density measure',
POSITIVE_RATIO_MEASURE(7850.),#1215);
#1222=MEASURE_REPRESENTATION_ITEM('density measure',
POSITIVE_RATIO_MEASURE(7850.),#1216);
#1223=MEASURE_REPRESENTATION_ITEM('density measure',
POSITIVE_RATIO_MEASURE(7850.),#1217);
#1224=PROPERTY_DEFINITION_REPRESENTATION(#1254,#1236);
#1225=PROPERTY_DEFINITION_REPRESENTATION(#1255,#1237);
#1226=PROPERTY_DEFINITION_REPRESENTATION(#1256,#1238);
#1227=PROPERTY_DEFINITION_REPRESENTATION(#1257,#1239);
#1228=PROPERTY_DEFINITION_REPRESENTATION(#1258,#1240);
#1229=PROPERTY_DEFINITION_REPRESENTATION(#1259,#1241);
#1230=PROPERTY_DEFINITION_REPRESENTATION(#1260,#1242);
#1231=PROPERTY_DEFINITION_REPRESENTATION(#1261,#1243);
#1232=PROPERTY_DEFINITION_REPRESENTATION(#1262,#1244);
#1233=PROPERTY_DEFINITION_REPRESENTATION(#1263,#1245);
#1234=PROPERTY_DEFINITION_REPRESENTATION(#1264,#1246);
#1235=PROPERTY_DEFINITION_REPRESENTATION(#1265,#1247);
#1236=REPRESENTATION('material name',(#1248),#2091);
#1237=REPRESENTATION('density',(#1218),#2091);
#1238=REPRESENTATION('material name',(#1249),#2092);
#1239=REPRESENTATION('density',(#1219),#2092);
#1240=REPRESENTATION('material name',(#1250),#2093);
#1241=REPRESENTATION('density',(#1220),#2093);
#1242=REPRESENTATION('material name',(#1251),#2094);
#1243=REPRESENTATION('density',(#1221),#2094);
#1244=REPRESENTATION('material name',(#1252),#2095);
#1245=REPRESENTATION('density',(#1222),#2095);
#1246=REPRESENTATION('material name',(#1253),#2096);
#1247=REPRESENTATION('density',(#1223),#2096);
#1248=DESCRIPTIVE_REPRESENTATION_ITEM('Steel','Steel');
#1249=DESCRIPTIVE_REPRESENTATION_ITEM('Steel','Steel');
#1250=DESCRIPTIVE_REPRESENTATION_ITEM('Steel','Steel');
#1251=DESCRIPTIVE_REPRESENTATION_ITEM('Steel','Steel');
#1252=DESCRIPTIVE_REPRESENTATION_ITEM('Steel','Steel');
#1253=DESCRIPTIVE_REPRESENTATION_ITEM('Steel','Steel');
#1254=PROPERTY_DEFINITION('material property','material name',#2154);
#1255=PROPERTY_DEFINITION('material property','density of part',#2154);
#1256=PROPERTY_DEFINITION('material property','material name',#2155);
#1257=PROPERTY_DEFINITION('material property','density of part',#2155);
#1258=PROPERTY_DEFINITION('material property','material name',#2156);
#1259=PROPERTY_DEFINITION('material property','density of part',#2156);
#1260=PROPERTY_DEFINITION('material property','material name',#2157);
#1261=PROPERTY_DEFINITION('material property','density of part',#2157);
#1262=PROPERTY_DEFINITION('material property','material name',#2158);
#1263=PROPERTY_DEFINITION('material property','density of part',#2158);
#1264=PROPERTY_DEFINITION('material property','material name',#2159);
#1265=PROPERTY_DEFINITION('material property','density of part',#2159);
#1266=AXIS2_PLACEMENT_3D('',#1750,#1388,#1389);
#1267=AXIS2_PLACEMENT_3D('',#1751,#1390,#1391);
#1268=AXIS2_PLACEMENT_3D('',#1752,#1392,#1393);
#1269=AXIS2_PLACEMENT_3D('',#1754,#1394,#1395);
#1270=AXIS2_PLACEMENT_3D('',#1757,#1397,#1398);
#1271=AXIS2_PLACEMENT_3D('',#1758,#1399,#1400);
#1272=AXIS2_PLACEMENT_3D('',#1759,#1401,#1402);
#1273=AXIS2_PLACEMENT_3D('',#1761,#1403,#1404);
#1274=AXIS2_PLACEMENT_3D('',#1764,#1406,#1407);
#1275=AXIS2_PLACEMENT_3D('',#1765,#1408,#1409);
#1276=AXIS2_PLACEMENT_3D('',#1766,#1410,#1411);
#1277=AXIS2_PLACEMENT_3D('',#1768,#1412,#1413);
#1278=AXIS2_PLACEMENT_3D('',#1771,#1415,#1416);
#1279=AXIS2_PLACEMENT_3D('',#1772,#1417,#1418);
#1280=AXIS2_PLACEMENT_3D('',#1773,#1419,#1420);
#1281=AXIS2_PLACEMENT_3D('',#1775,#1421,#1422);
#1282=AXIS2_PLACEMENT_3D('',#1778,#1424,#1425);
#1283=AXIS2_PLACEMENT_3D('',#1779,#1426,#1427);
#1284=AXIS2_PLACEMENT_3D('',#1780,#1428,#1429);
#1285=AXIS2_PLACEMENT_3D('',#1782,#1430,#1431);
#1286=AXIS2_PLACEMENT_3D('',#1785,#1433,#1434);
#1287=AXIS2_PLACEMENT_3D('',#1786,#1435,#1436);
#1288=AXIS2_PLACEMENT_3D('',#1787,#1437,#1438);
#1289=AXIS2_PLACEMENT_3D('',#1789,#1439,#1440);
#1290=AXIS2_PLACEMENT_3D('',#1792,#1442,#1443);
#1291=AXIS2_PLACEMENT_3D('',#1793,#1444,#1445);
#1292=AXIS2_PLACEMENT_3D('',#1794,#1446,#1447);
#1293=AXIS2_PLACEMENT_3D('',#1803,#1452,#1453);
#1294=AXIS2_PLACEMENT_3D('',#1812,#1458,#1459);
#1295=AXIS2_PLACEMENT_3D('',#1821,#1464,#1465);
#1296=AXIS2_PLACEMENT_3D('',#1830,#1470,#1471);
#1297=AXIS2_PLACEMENT_3D('',#1859,#1488,#1489);
#1298=AXIS2_PLACEMENT_3D('',#1863,#1492,#1493);
#1299=AXIS2_PLACEMENT_3D('',#1867,#1496,#1497);
#1300=AXIS2_PLACEMENT_3D('',#1871,#1500,#1501);
#1301=AXIS2_PLACEMENT_3D('',#1875,#1504,#1505);
#1302=AXIS2_PLACEMENT_3D('',#1877,#1507,#1508);
#1303=AXIS2_PLACEMENT_3D('',#1879,#1510,#1511);
#1304=AXIS2_PLACEMENT_3D('',#1883,#1514,#1515);
#1305=AXIS2_PLACEMENT_3D('',#1887,#1518,#1519);
#1306=AXIS2_PLACEMENT_3D('',#1891,#1522,#1523);
#1307=AXIS2_PLACEMENT_3D('',#1895,#1526,#1527);
#1308=AXIS2_PLACEMENT_3D('',#1897,#1529,#1530);
#1309=AXIS2_PLACEMENT_3D('',#1899,#1532,#1533);
#1310=AXIS2_PLACEMENT_3D('',#1905,#1537,#1538);
#1311=AXIS2_PLACEMENT_3D('',#1909,#1541,#1542);
#1312=AXIS2_PLACEMENT_3D('',#1913,#1545,#1546);
#1313=AXIS2_PLACEMENT_3D('',#1915,#1548,#1549);
#1314=AXIS2_PLACEMENT_3D('',#1916,#1550,#1551);
#1315=AXIS2_PLACEMENT_3D('',#1917,#1552,#1553);
#1316=AXIS2_PLACEMENT_3D('',#1926,#1558,#1559);
#1317=AXIS2_PLACEMENT_3D('',#1935,#1564,#1565);
#1318=AXIS2_PLACEMENT_3D('',#1938,#1568,#1569);
#1319=AXIS2_PLACEMENT_3D('',#1948,#1575,#1576);
#1320=AXIS2_PLACEMENT_3D('',#1952,#1579,#1580);
#1321=AXIS2_PLACEMENT_3D('',#1958,#1584,#1585);
#1322=AXIS2_PLACEMENT_3D('',#1962,#1588,#1589);
#1323=AXIS2_PLACEMENT_3D('',#1965,#1592,#1593);
#1324=AXIS2_PLACEMENT_3D('',#1966,#1594,#1595);
#1325=AXIS2_PLACEMENT_3D('',#1967,#1596,#1597);
#1326=AXIS2_PLACEMENT_3D('',#1968,#1598,#1599);
#1327=AXIS2_PLACEMENT_3D('',#1977,#1604,#1605);
#1328=AXIS2_PLACEMENT_3D('',#1983,#1609,#1610);
#1329=AXIS2_PLACEMENT_3D('',#1989,#1614,#1615);
#1330=AXIS2_PLACEMENT_3D('',#1992,#1618,#1619);
#1331=AXIS2_PLACEMENT_3D('',#1993,#1620,#1621);
#1332=AXIS2_PLACEMENT_3D('',#1994,#1622,#1623);
#1333=AXIS2_PLACEMENT_3D('',#1995,#1624,#1625);
#1334=AXIS2_PLACEMENT_3D('',#2004,#1630,#1631);
#1335=AXIS2_PLACEMENT_3D('',#2010,#1635,#1636);
#1336=AXIS2_PLACEMENT_3D('',#2016,#1640,#1641);
#1337=AXIS2_PLACEMENT_3D('',#2019,#1644,#1645);
#1338=AXIS2_PLACEMENT_3D('',#2020,#1646,#1647);
#1339=AXIS2_PLACEMENT_3D('',#2021,#1648,#1649);
#1340=AXIS2_PLACEMENT_3D('',#2022,#1650,#1651);
#1341=AXIS2_PLACEMENT_3D('',#2024,#1652,#1653);
#1342=AXIS2_PLACEMENT_3D('',#2027,#1655,#1656);
#1343=AXIS2_PLACEMENT_3D('',#2028,#1657,#1658);
#1344=AXIS2_PLACEMENT_3D('',#2029,#1659,#1660);
#1345=AXIS2_PLACEMENT_3D('',#2031,#1661,#1662);
#1346=AXIS2_PLACEMENT_3D('',#2034,#1664,#1665);
#1347=AXIS2_PLACEMENT_3D('',#2035,#1666,#1667);
#1348=AXIS2_PLACEMENT_3D('',#2036,#1668,#1669);
#1349=AXIS2_PLACEMENT_3D('',#2038,#1670,#1671);
#1350=AXIS2_PLACEMENT_3D('',#2041,#1673,#1674);
#1351=AXIS2_PLACEMENT_3D('',#2042,#1675,#1676);
#1352=AXIS2_PLACEMENT_3D('',#2043,#1677,#1678);
#1353=AXIS2_PLACEMENT_3D('',#2044,#1679,#1680);
#1354=AXIS2_PLACEMENT_3D('',#2045,#1681,#1682);
#1355=AXIS2_PLACEMENT_3D('',#2047,#1683,#1684);
#1356=AXIS2_PLACEMENT_3D('',#2050,#1686,#1687);
#1357=AXIS2_PLACEMENT_3D('',#2051,#1688,#1689);
#1358=AXIS2_PLACEMENT_3D('',#2052,#1690,#1691);
#1359=AXIS2_PLACEMENT_3D('',#2053,#1692,#1693);
#1360=AXIS2_PLACEMENT_3D('',#2054,#1694,#1695);
#1361=AXIS2_PLACEMENT_3D('',#2055,#1696,#1697);
#1362=AXIS2_PLACEMENT_3D('',#2056,#1698,#1699);
#1363=AXIS2_PLACEMENT_3D('',#2057,#1700,#1701);
#1364=AXIS2_PLACEMENT_3D('',#2058,#1702,#1703);
#1365=AXIS2_PLACEMENT_3D('',#2059,#1704,#1705);
#1366=AXIS2_PLACEMENT_3D('',#2060,#1706,#1707);
#1367=AXIS2_PLACEMENT_3D('',#2061,#1708,#1709);
#1368=AXIS2_PLACEMENT_3D('',#2062,#1710,#1711);
#1369=AXIS2_PLACEMENT_3D('',#2063,#1712,#1713);
#1370=AXIS2_PLACEMENT_3D('',#2064,#1714,#1715);
#1371=AXIS2_PLACEMENT_3D('',#2065,#1716,#1717);
#1372=AXIS2_PLACEMENT_3D('',#2066,#1718,#1719);
#1373=AXIS2_PLACEMENT_3D('',#2067,#1720,#1721);
#1374=AXIS2_PLACEMENT_3D('',#2068,#1722,#1723);
#1375=AXIS2_PLACEMENT_3D('',#2069,#1724,#1725);
#1376=AXIS2_PLACEMENT_3D('',#2070,#1726,#1727);
#1377=AXIS2_PLACEMENT_3D('',#2071,#1728,#1729);
#1378=AXIS2_PLACEMENT_3D('',#2072,#1730,#1731);
#1379=AXIS2_PLACEMENT_3D('',#2073,#1732,#1733);
#1380=AXIS2_PLACEMENT_3D('',#2074,#1734,#1735);
#1381=AXIS2_PLACEMENT_3D('',#2075,#1736,#1737);
#1382=AXIS2_PLACEMENT_3D('',#2076,#1738,#1739);
#1383=AXIS2_PLACEMENT_3D('',#2077,#1740,#1741);
#1384=AXIS2_PLACEMENT_3D('',#2078,#1742,#1743);
#1385=AXIS2_PLACEMENT_3D('',#2079,#1744,#1745);
#1386=AXIS2_PLACEMENT_3D('',#2080,#1746,#1747);
#1387=AXIS2_PLACEMENT_3D('',#2081,#1748,#1749);
#1388=DIRECTION('axis',(0.,0.,1.));
#1389=DIRECTION('refdir',(1.,0.,0.));
#1390=DIRECTION('axis',(0.,0.,1.));
#1391=DIRECTION('refdir',(1.,0.,0.));
#1392=DIRECTION('center_axis',(1.,0.,0.));
#1393=DIRECTION('ref_axis',(0.,0.,-1.));
#1394=DIRECTION('center_axis',(1.,0.,0.));
#1395=DIRECTION('ref_axis',(0.,0.,-1.));
#1396=DIRECTION('',(1.,0.,0.));
#1397=DIRECTION('center_axis',(1.,0.,0.));
#1398=DIRECTION('ref_axis',(0.,0.,-1.));
#1399=DIRECTION('center_axis',(1.,0.,0.));
#1400=DIRECTION('ref_axis',(0.,0.,-1.));
#1401=DIRECTION('center_axis',(1.,0.,0.));
#1402=DIRECTION('ref_axis',(0.,0.,-1.));
#1403=DIRECTION('center_axis',(1.,0.,0.));
#1404=DIRECTION('ref_axis',(0.,0.,-1.));
#1405=DIRECTION('',(1.,0.,0.));
#1406=DIRECTION('center_axis',(1.,0.,0.));
#1407=DIRECTION('ref_axis',(0.,0.,-1.));
#1408=DIRECTION('center_axis',(1.,0.,0.));
#1409=DIRECTION('ref_axis',(0.,0.,-1.));
#1410=DIRECTION('center_axis',(1.,0.,0.));
#1411=DIRECTION('ref_axis',(0.,0.,-1.));
#1412=DIRECTION('center_axis',(1.,0.,0.));
#1413=DIRECTION('ref_axis',(0.,0.,-1.));
#1414=DIRECTION('',(1.,0.,0.));
#1415=DIRECTION('center_axis',(1.,0.,0.));
#1416=DIRECTION('ref_axis',(0.,0.,-1.));
#1417=DIRECTION('center_axis',(1.,0.,0.));
#1418=DIRECTION('ref_axis',(0.,0.,-1.));
#1419=DIRECTION('center_axis',(1.,0.,0.));
#1420=DIRECTION('ref_axis',(0.,0.,-1.));
#1421=DIRECTION('center_axis',(1.,0.,0.));
#1422=DIRECTION('ref_axis',(0.,0.,-1.));
#1423=DIRECTION('',(1.,0.,0.));
#1424=DIRECTION('center_axis',(1.,0.,0.));
#1425=DIRECTION('ref_axis',(0.,0.,-1.));
#1426=DIRECTION('center_axis',(1.,0.,0.));
#1427=DIRECTION('ref_axis',(0.,0.,-1.));
#1428=DIRECTION('center_axis',(-1.,0.,0.));
#1429=DIRECTION('ref_axis',(0.,0.,-1.));
#1430=DIRECTION('center_axis',(-1.,0.,0.));
#1431=DIRECTION('ref_axis',(0.,0.,-1.));
#1432=DIRECTION('',(-1.,0.,0.));
#1433=DIRECTION('center_axis',(-1.,0.,0.));
#1434=DIRECTION('ref_axis',(0.,0.,-1.));
#1435=DIRECTION('center_axis',(1.,0.,0.));
#1436=DIRECTION('ref_axis',(0.,0.,-1.));
#1437=DIRECTION('center_axis',(-1.,0.,0.));
#1438=DIRECTION('ref_axis',(0.,0.,-1.));
#1439=DIRECTION('center_axis',(-1.,0.,0.));
#1440=DIRECTION('ref_axis',(0.,0.,-1.));
#1441=DIRECTION('',(-1.,0.,0.));
#1442=DIRECTION('center_axis',(-1.,0.,0.));
#1443=DIRECTION('ref_axis',(0.,0.,-1.));
#1444=DIRECTION('center_axis',(1.,0.,0.));
#1445=DIRECTION('ref_axis',(0.,0.,-1.));
#1446=DIRECTION('center_axis',(0.,1.,0.));
#1447=DIRECTION('ref_axis',(-1.,0.,0.));
#1448=DIRECTION('',(1.,0.,0.));
#1449=DIRECTION('',(0.,0.,1.));
#1450=DIRECTION('',(-1.,0.,0.));
#1451=DIRECTION('',(0.,0.,-1.));
#1452=DIRECTION('center_axis',(0.,1.,0.));
#1453=DIRECTION('ref_axis',(-1.,0.,0.));
#1454=DIRECTION('',(1.,0.,0.));
#1455=DIRECTION('',(0.,0.,1.));
#1456=DIRECTION('',(-1.,0.,0.));
#1457=DIRECTION('',(0.,0.,-1.));
#1458=DIRECTION('center_axis',(0.,-1.,0.));
#1459=DIRECTION('ref_axis',(1.,0.,0.));
#1460=DIRECTION('',(-1.,0.,0.));
#1461=DIRECTION('',(0.,0.,1.));
#1462=DIRECTION('',(1.,0.,0.));
#1463=DIRECTION('',(0.,0.,1.));
#1464=DIRECTION('center_axis',(0.,-1.,0.));
#1465=DIRECTION('ref_axis',(1.,0.,0.));
#1466=DIRECTION('',(-1.,0.,0.));
#1467=DIRECTION('',(0.,0.,1.));
#1468=DIRECTION('',(1.,0.,0.));
#1469=DIRECTION('',(0.,0.,1.));
#1470=DIRECTION('center_axis',(-1.,0.,0.));
#1471=DIRECTION('ref_axis',(0.,-1.,0.));
#1472=DIRECTION('',(0.,-1.,0.));
#1473=DIRECTION('',(0.,0.,-1.));
#1474=DIRECTION('',(0.,1.,0.));
#1475=DIRECTION('',(0.,0.,1.));
#1476=DIRECTION('',(0.,-1.,0.));
#1477=DIRECTION('',(0.,-1.,0.));
#1478=DIRECTION('',(0.,0.,1.));
#1479=DIRECTION('',(0.,-1.,0.));
#1480=DIRECTION('',(0.,-1.,0.));
#1481=DIRECTION('',(0.,0.,1.));
#1482=DIRECTION('',(0.,-1.,0.));
#1483=DIRECTION('',(0.,0.,-1.));
#1484=DIRECTION('',(0.,-1.,0.));
#1485=DIRECTION('',(0.,-1.,0.));
#1486=DIRECTION('',(0.,0.,-1.));
#1487=DIRECTION('',(0.,-1.,0.));
#1488=DIRECTION('center_axis',(0.,0.,1.));
#1489=DIRECTION('ref_axis',(1.,0.,0.));
#1490=DIRECTION('',(-1.,0.,0.));
#1491=DIRECTION('',(0.,-1.,0.));
#1492=DIRECTION('center_axis',(0.,0.,1.));
#1493=DIRECTION('ref_axis',(1.,0.,0.));
#1494=DIRECTION('',(0.,-1.,0.));
#1495=DIRECTION('',(1.,0.,0.));
#1496=DIRECTION('center_axis',(1.,0.,0.));
#1497=DIRECTION('ref_axis',(0.,1.,0.));
#1498=DIRECTION('',(0.,0.,1.));
#1499=DIRECTION('',(0.,1.,0.));
#1500=DIRECTION('center_axis',(1.,0.,0.));
#1501=DIRECTION('ref_axis',(0.,1.,0.));
#1502=DIRECTION('',(0.,1.,0.));
#1503=DIRECTION('',(0.,0.,1.));
#1504=DIRECTION('center_axis',(0.,0.,1.));
#1505=DIRECTION('ref_axis',(1.,0.,0.));
#1506=DIRECTION('',(1.,0.,0.));
#1507=DIRECTION('center_axis',(0.,0.,1.));
#1508=DIRECTION('ref_axis',(1.,0.,0.));
#1509=DIRECTION('',(-1.,0.,0.));
#1510=DIRECTION('center_axis',(0.,0.,1.));
#1511=DIRECTION('ref_axis',(1.,0.,0.));
#1512=DIRECTION('',(-1.,0.,0.));
#1513=DIRECTION('',(0.,-1.,0.));
#1514=DIRECTION('center_axis',(0.,0.,1.));
#1515=DIRECTION('ref_axis',(1.,0.,0.));
#1516=DIRECTION('',(0.,-1.,0.));
#1517=DIRECTION('',(1.,0.,0.));
#1518=DIRECTION('center_axis',(1.,0.,0.));
#1519=DIRECTION('ref_axis',(0.,1.,0.));
#1520=DIRECTION('',(0.,0.,1.));
#1521=DIRECTION('',(0.,1.,0.));
#1522=DIRECTION('center_axis',(1.,0.,0.));
#1523=DIRECTION('ref_axis',(0.,1.,0.));
#1524=DIRECTION('',(0.,1.,0.));
#1525=DIRECTION('',(0.,0.,1.));
#1526=DIRECTION('center_axis',(0.,0.,1.));
#1527=DIRECTION('ref_axis',(1.,0.,0.));
#1528=DIRECTION('',(1.,0.,0.));
#1529=DIRECTION('center_axis',(0.,0.,1.));
#1530=DIRECTION('ref_axis',(1.,0.,0.));
#1531=DIRECTION('',(-1.,0.,0.));
#1532=DIRECTION('center_axis',(0.,1.,0.));
#1533=DIRECTION('ref_axis',(-1.,0.,0.));
#1534=DIRECTION('',(-1.,0.,0.));
#1535=DIRECTION('',(0.,0.,1.));
#1536=DIRECTION('',(-1.,0.,0.));
#1537=DIRECTION('center_axis',(0.,0.,1.));
#1538=DIRECTION('ref_axis',(1.,0.,0.));
#1539=DIRECTION('',(1.,0.,0.));
#1540=DIRECTION('',(0.,-1.,0.));
#1541=DIRECTION('center_axis',(0.,-1.,0.));
#1542=DIRECTION('ref_axis',(1.,0.,0.));
#1543=DIRECTION('',(1.,0.,0.));
#1544=DIRECTION('',(0.,0.,1.));
#1545=DIRECTION('center_axis',(-1.,0.,0.));
#1546=DIRECTION('ref_axis',(0.,-1.,0.));
#1547=DIRECTION('',(0.,-1.,0.));
#1548=DIRECTION('center_axis',(0.,0.,1.));
#1549=DIRECTION('ref_axis',(1.,0.,0.));
#1550=DIRECTION('axis',(0.,0.,1.));
#1551=DIRECTION('refdir',(1.,0.,0.));
#1552=DIRECTION('center_axis',(0.,-1.,0.));
#1553=DIRECTION('ref_axis',(1.,0.,0.));
#1554=DIRECTION('',(-1.,0.,0.));
#1555=DIRECTION('',(0.,0.,1.));
#1556=DIRECTION('',(1.,0.,0.));
#1557=DIRECTION('',(0.,0.,-1.));
#1558=DIRECTION('center_axis',(0.,1.,0.));
#1559=DIRECTION('ref_axis',(-1.,0.,0.));
#1560=DIRECTION('',(1.,0.,0.));
#1561=DIRECTION('',(0.,0.,1.));
#1562=DIRECTION('',(-1.,0.,0.));
#1563=DIRECTION('',(0.,0.,-1.));
#1564=DIRECTION('center_axis',(0.,0.,1.));
#1565=DIRECTION('ref_axis',(1.,0.,0.));
#1566=DIRECTION('',(0.,1.,0.));
#1567=DIRECTION('',(0.,-1.,0.));
#1568=DIRECTION('center_axis',(1.,0.,0.));
#1569=DIRECTION('ref_axis',(0.,1.,0.));
#1570=DIRECTION('',(0.,1.,0.));
#1571=DIRECTION('',(0.,0.,1.));
#1572=DIRECTION('',(0.,1.,0.));
#1573=DIRECTION('',(0.,0.,1.));
#1574=DIRECTION('',(0.,1.,0.));
#1575=DIRECTION('center_axis',(0.,0.,1.));
#1576=DIRECTION('ref_axis',(1.,0.,0.));
#1577=DIRECTION('',(0.,-1.,0.));
#1578=DIRECTION('',(1.,0.,0.));
#1579=DIRECTION('center_axis',(0.,1.,0.));
#1580=DIRECTION('ref_axis',(-1.,0.,0.));
#1581=DIRECTION('',(-1.,0.,0.));
#1582=DIRECTION('',(0.,0.,1.));
#1583=DIRECTION('',(-1.,0.,0.));
#1584=DIRECTION('center_axis',(0.,-1.,0.));
#1585=DIRECTION('ref_axis',(1.,0.,0.));
#1586=DIRECTION('',(1.,0.,0.));
#1587=DIRECTION('',(0.,0.,1.));
#1588=DIRECTION('center_axis',(-1.,0.,0.));
#1589=DIRECTION('ref_axis',(0.,-1.,0.));
#1590=DIRECTION('',(0.,-1.,0.));
#1591=DIRECTION('',(0.,-1.,0.));
#1592=DIRECTION('center_axis',(0.,0.,1.));
#1593=DIRECTION('ref_axis',(1.,0.,0.));
#1594=DIRECTION('center_axis',(0.,0.,1.));
#1595=DIRECTION('ref_axis',(1.,0.,0.));
#1596=DIRECTION('axis',(0.,0.,1.));
#1597=DIRECTION('refdir',(1.,0.,0.));
#1598=DIRECTION('center_axis',(0.,1.,0.));
#1599=DIRECTION('ref_axis',(-1.,0.,0.));
#1600=DIRECTION('',(-1.,0.,0.));
#1601=DIRECTION('',(0.,0.,1.));
#1602=DIRECTION('',(-1.,0.,0.));
#1603=DIRECTION('',(0.,0.,1.));
#1604=DIRECTION('center_axis',(1.,0.,0.));
#1605=DIRECTION('ref_axis',(0.,1.,0.));
#1606=DIRECTION('',(0.,1.,0.));
#1607=DIRECTION('',(0.,1.,0.));
#1608=DIRECTION('',(0.,0.,1.));
#1609=DIRECTION('center_axis',(0.,-1.,0.));
#1610=DIRECTION('ref_axis',(1.,0.,0.));
#1611=DIRECTION('',(1.,0.,0.));
#1612=DIRECTION('',(1.,0.,0.));
#1613=DIRECTION('',(0.,0.,1.));
#1614=DIRECTION('center_axis',(-1.,0.,0.));
#1615=DIRECTION('ref_axis',(0.,-1.,0.));
#1616=DIRECTION('',(0.,-1.,0.));
#1617=DIRECTION('',(0.,-1.,0.));
#1618=DIRECTION('center_axis',(0.,0.,1.));
#1619=DIRECTION('ref_axis',(1.,0.,0.));
#1620=DIRECTION('center_axis',(0.,0.,1.));
#1621=DIRECTION('ref_axis',(1.,0.,0.));
#1622=DIRECTION('axis',(0.,0.,1.));
#1623=DIRECTION('refdir',(1.,0.,0.));
#1624=DIRECTION('center_axis',(0.,1.,0.));
#1625=DIRECTION('ref_axis',(-1.,0.,0.));
#1626=DIRECTION('',(-1.,0.,0.));
#1627=DIRECTION('',(0.,0.,1.));
#1628=DIRECTION('',(-1.,0.,0.));
#1629=DIRECTION('',(0.,0.,1.));
#1630=DIRECTION('center_axis',(1.,0.,0.));
#1631=DIRECTION('ref_axis',(0.,1.,0.));
#1632=DIRECTION('',(0.,1.,0.));
#1633=DIRECTION('',(0.,1.,0.));
#1634=DIRECTION('',(0.,0.,1.));
#1635=DIRECTION('center_axis',(0.,-1.,0.));
#1636=DIRECTION('ref_axis',(1.,0.,0.));
#1637=DIRECTION('',(1.,0.,0.));
#1638=DIRECTION('',(1.,0.,0.));
#1639=DIRECTION('',(0.,0.,1.));
#1640=DIRECTION('center_axis',(-1.,0.,0.));
#1641=DIRECTION('ref_axis',(0.,-1.,0.));
#1642=DIRECTION('',(0.,-1.,0.));
#1643=DIRECTION('',(0.,-1.,0.));
#1644=DIRECTION('center_axis',(0.,0.,1.));
#1645=DIRECTION('ref_axis',(1.,0.,0.));
#1646=DIRECTION('center_axis',(0.,0.,1.));
#1647=DIRECTION('ref_axis',(1.,0.,0.));
#1648=DIRECTION('axis',(0.,0.,1.));
#1649=DIRECTION('refdir',(1.,0.,0.));
#1650=DIRECTION('center_axis',(0.,0.,1.));
#1651=DIRECTION('ref_axis',(1.,0.,0.));
#1652=DIRECTION('center_axis',(0.,0.,1.));
#1653=DIRECTION('ref_axis',(1.,0.,0.));
#1654=DIRECTION('',(0.,0.,-1.));
#1655=DIRECTION('center_axis',(0.,0.,-1.));
#1656=DIRECTION('ref_axis',(1.,0.,0.));
#1657=DIRECTION('center_axis',(0.,0.,1.));
#1658=DIRECTION('ref_axis',(1.,0.,0.));
#1659=DIRECTION('center_axis',(0.,0.,1.));
#1660=DIRECTION('ref_axis',(1.,0.,0.));
#1661=DIRECTION('center_axis',(0.,0.,1.));
#1662=DIRECTION('ref_axis',(1.,0.,0.));
#1663=DIRECTION('',(0.,0.,-1.));
#1664=DIRECTION('center_axis',(0.,0.,1.));
#1665=DIRECTION('ref_axis',(1.,0.,0.));
#1666=DIRECTION('center_axis',(0.,0.,1.));
#1667=DIRECTION('ref_axis',(1.,0.,0.));
#1668=DIRECTION('center_axis',(0.,0.,1.));
#1669=DIRECTION('ref_axis',(1.,0.,0.));
#1670=DIRECTION('center_axis',(0.,0.,1.));
#1671=DIRECTION('ref_axis',(1.,0.,0.));
#1672=DIRECTION('',(0.,0.,-1.));
#1673=DIRECTION('center_axis',(0.,0.,1.));
#1674=DIRECTION('ref_axis',(1.,0.,0.));
#1675=DIRECTION('center_axis',(0.,0.,1.));
#1676=DIRECTION('ref_axis',(1.,0.,0.));
#1677=DIRECTION('center_axis',(0.,0.,1.));
#1678=DIRECTION('ref_axis',(1.,0.,0.));
#1679=DIRECTION('axis',(0.,0.,1.));
#1680=DIRECTION('refdir',(1.,0.,0.));
#1681=DIRECTION('center_axis',(0.,0.,1.));
#1682=DIRECTION('ref_axis',(1.,0.,0.));
#1683=DIRECTION('center_axis',(0.,0.,1.));
#1684=DIRECTION('ref_axis',(1.,0.,0.));
#1685=DIRECTION('',(0.,0.,-1.));
#1686=DIRECTION('center_axis',(0.,0.,1.));
#1687=DIRECTION('ref_axis',(1.,0.,0.));
#1688=DIRECTION('center_axis',(0.,0.,1.));
#1689=DIRECTION('ref_axis',(1.,0.,0.));
#1690=DIRECTION('center_axis',(0.,0.,1.));
#1691=DIRECTION('ref_axis',(1.,0.,0.));
#1692=DIRECTION('',(0.,0.,1.));
#1693=DIRECTION('',(1.,0.,0.));
#1694=DIRECTION('',(0.,0.,1.));
#1695=DIRECTION('',(1.,0.,0.));
#1696=DIRECTION('',(0.,0.,1.));
#1697=DIRECTION('',(1.,0.,0.));
#1698=DIRECTION('',(0.,0.,1.));
#1699=DIRECTION('',(1.,0.,0.));
#1700=DIRECTION('',(1.,0.,2.22044604925031E-16));
#1701=DIRECTION('',(2.22044604925031E-16,0.,-1.));
#1702=DIRECTION('',(1.,0.,2.22044604925031E-16));
#1703=DIRECTION('',(2.22044604925031E-16,0.,-1.));
#1704=DIRECTION('',(1.22464679914735E-16,0.,-1.));
#1705=DIRECTION('',(-1.,0.,-1.22464679914735E-16));
#1706=DIRECTION('',(1.22464679914735E-16,0.,-1.));
#1707=DIRECTION('',(-1.,0.,-1.22464679914735E-16));
#1708=DIRECTION('',(0.,0.,1.));
#1709=DIRECTION('',(1.,0.,0.));
#1710=DIRECTION('',(1.22464679914735E-16,0.,-1.));
#1711=DIRECTION('',(-1.,0.,-1.22464679914735E-16));
#1712=DIRECTION('',(0.,0.,1.));
#1713=DIRECTION('',(1.,0.,0.));
#1714=DIRECTION('',(1.22464679914735E-16,0.,-1.));
#1715=DIRECTION('',(-1.,0.,-1.22464679914735E-16));
#1716=DIRECTION('',(0.,0.,1.));
#1717=DIRECTION('',(1.,0.,0.));
#1718=DIRECTION('',(0.,0.,1.));
#1719=DIRECTION('',(1.,0.,0.));
#1720=DIRECTION('',(1.,0.,2.22044604925031E-16));
#1721=DIRECTION('',(2.22044604925031E-16,0.,-1.));
#1722=DIRECTION('',(0.,0.,1.));
#1723=DIRECTION('',(1.,0.,0.));
#1724=DIRECTION('',(1.22464679914735E-16,0.,-1.));
#1725=DIRECTION('',(-1.,0.,-1.22464679914735E-16));
#1726=DIRECTION('',(0.,0.,1.));
#1727=DIRECTION('',(1.,0.,0.));
#1728=DIRECTION('',(1.22464679914735E-16,0.,-1.));
#1729=DIRECTION('',(-1.,0.,-1.22464679914735E-16));
#1730=DIRECTION('',(0.,0.,1.));
#1731=DIRECTION('',(1.,0.,0.));
#1732=DIRECTION('',(0.,0.,1.));
#1733=DIRECTION('',(1.,0.,0.));
#1734=DIRECTION('',(1.,0.,2.22044604925031E-16));
#1735=DIRECTION('',(2.22044604925031E-16,0.,-1.));
#1736=DIRECTION('',(1.,0.,2.22044604925031E-16));
#1737=DIRECTION('',(2.22044604925031E-16,0.,-1.));
#1738=DIRECTION('',(1.,0.,2.22044604925031E-16));
#1739=DIRECTION('',(2.22044604925031E-16,0.,-1.));
#1740=DIRECTION('',(1.,0.,2.22044604925031E-16));
#1741=DIRECTION('',(2.22044604925031E-16,0.,-1.));
#1742=DIRECTION('',(1.,0.,2.22044604925031E-16));
#1743=DIRECTION('',(2.22044604925031E-16,0.,-1.));
#1744=DIRECTION('',(1.,0.,2.22044604925031E-16));
#1745=DIRECTION('',(2.22044604925031E-16,0.,-1.));
#1746=DIRECTION('',(1.,0.,2.22044604925031E-16));
#1747=DIRECTION('',(2.22044604925031E-16,0.,-1.));
#1748=DIRECTION('',(1.,0.,2.22044604925031E-16));
#1749=DIRECTION('',(2.22044604925031E-16,0.,-1.));
#1750=CARTESIAN_POINT('',(0.,0.,0.));
#1751=CARTESIAN_POINT('',(0.,0.,0.));
#1752=CARTESIAN_POINT('Origin',(0.,51.,60.));
#1753=CARTESIAN_POINT('',(0.,51.,60.41));
#1754=CARTESIAN_POINT('Origin',(0.,51.,60.));
#1755=CARTESIAN_POINT('',(1.5,51.,60.41));
#1756=CARTESIAN_POINT('',(0.,51.,60.41));
#1757=CARTESIAN_POINT('Origin',(1.5,51.,60.));
#1758=CARTESIAN_POINT('Origin',(1.5,51.,60.));
#1759=CARTESIAN_POINT('Origin',(0.,9.,120.));
#1760=CARTESIAN_POINT('',(0.,9.,120.41));
#1761=CARTESIAN_POINT('Origin',(0.,9.,120.));
#1762=CARTESIAN_POINT('',(1.5,9.,120.41));
#1763=CARTESIAN_POINT('',(0.,9.,120.41));
#1764=CARTESIAN_POINT('Origin',(1.5,9.,120.));
#1765=CARTESIAN_POINT('Origin',(1.5,9.,120.));
#1766=CARTESIAN_POINT('Origin',(0.,9.,60.));
#1767=CARTESIAN_POINT('',(0.,9.,60.41));
#1768=CARTESIAN_POINT('Origin',(0.,9.,60.));
#1769=CARTESIAN_POINT('',(1.5,9.,60.41));
#1770=CARTESIAN_POINT('',(0.,9.,60.41));
#1771=CARTESIAN_POINT('Origin',(1.5,9.,60.));
#1772=CARTESIAN_POINT('Origin',(1.5,9.,60.));
#1773=CARTESIAN_POINT('Origin',(0.,51.,120.));
#1774=CARTESIAN_POINT('',(0.,51.,120.41));
#1775=CARTESIAN_POINT('Origin',(0.,51.,120.));
#1776=CARTESIAN_POINT('',(1.5,51.,120.41));
#1777=CARTESIAN_POINT('',(0.,51.,120.41));
#1778=CARTESIAN_POINT('Origin',(1.5,51.,120.));
#1779=CARTESIAN_POINT('Origin',(1.5,51.,120.));
#1780=CARTESIAN_POINT('Origin',(1.8,30.,18.));
#1781=CARTESIAN_POINT('',(1.8,30.,18.62));
#1782=CARTESIAN_POINT('Origin',(1.8,30.,18.));
#1783=CARTESIAN_POINT('',(1.18,30.,18.62));
#1784=CARTESIAN_POINT('',(1.8,30.,18.62));
#1785=CARTESIAN_POINT('Origin',(1.18,30.,18.));
#1786=CARTESIAN_POINT('Origin',(1.18,30.,18.));
#1787=CARTESIAN_POINT('Origin',(1.8,30.,162.));
#1788=CARTESIAN_POINT('',(1.8,30.,162.62));
#1789=CARTESIAN_POINT('Origin',(1.8,30.,162.));
#1790=CARTESIAN_POINT('',(1.18,30.,162.62));
#1791=CARTESIAN_POINT('',(1.8,30.,162.62));
#1792=CARTESIAN_POINT('Origin',(1.18,30.,162.));
#1793=CARTESIAN_POINT('Origin',(1.18,30.,162.));
#1794=CARTESIAN_POINT('Origin',(1.81,58.82,0.));
#1795=CARTESIAN_POINT('',(1.3,58.82,89.08));
#1796=CARTESIAN_POINT('',(1.8,58.82,89.08));
#1797=CARTESIAN_POINT('',(1.6825,58.82,89.08));
#1798=CARTESIAN_POINT('',(1.3,58.82,1.82));
#1799=CARTESIAN_POINT('',(1.3,58.82,0.));
#1800=CARTESIAN_POINT('',(1.8,58.82,1.82));
#1801=CARTESIAN_POINT('',(1.6825,58.82,1.82));
#1802=CARTESIAN_POINT('',(1.8,58.82,0.));
#1803=CARTESIAN_POINT('Origin',(1.81,58.82,0.));
#1804=CARTESIAN_POINT('',(1.3,58.82,178.18));
#1805=CARTESIAN_POINT('',(1.8,58.82,178.18));
#1806=CARTESIAN_POINT('',(1.6825,58.82,178.18));
#1807=CARTESIAN_POINT('',(1.3,58.82,90.92));
#1808=CARTESIAN_POINT('',(1.3,58.82,0.));
#1809=CARTESIAN_POINT('',(1.8,58.82,90.92));
#1810=CARTESIAN_POINT('',(1.6825,58.82,90.92));
#1811=CARTESIAN_POINT('',(1.8,58.82,0.));
#1812=CARTESIAN_POINT('Origin',(1.3,58.18,0.));
#1813=CARTESIAN_POINT('',(1.8,58.18,89.08));
#1814=CARTESIAN_POINT('',(1.3,58.18,89.08));
#1815=CARTESIAN_POINT('',(1.4275,58.18,89.08));
#1816=CARTESIAN_POINT('',(1.8,58.18,1.82));
#1817=CARTESIAN_POINT('',(1.8,58.18,0.));
#1818=CARTESIAN_POINT('',(1.3,58.18,1.82));
#1819=CARTESIAN_POINT('',(1.4275,58.18,1.82));
#1820=CARTESIAN_POINT('',(1.3,58.18,0.));
#1821=CARTESIAN_POINT('Origin',(1.3,58.18,0.));
#1822=CARTESIAN_POINT('',(1.8,58.18,178.18));
#1823=CARTESIAN_POINT('',(1.3,58.18,178.18));
#1824=CARTESIAN_POINT('',(1.4275,58.18,178.18));
#1825=CARTESIAN_POINT('',(1.8,58.18,90.92));
#1826=CARTESIAN_POINT('',(1.8,58.18,0.));
#1827=CARTESIAN_POINT('',(1.3,58.18,90.92));
#1828=CARTESIAN_POINT('',(1.4275,58.18,90.92));
#1829=CARTESIAN_POINT('',(1.3,58.18,0.));
#1830=CARTESIAN_POINT('Origin',(1.3,60.,178.18));
#1831=CARTESIAN_POINT('',(1.3,60.,178.18));
#1832=CARTESIAN_POINT('',(1.3,60.,178.18));
#1833=CARTESIAN_POINT('',(1.3,60.,180.));
#1834=CARTESIAN_POINT('',(1.3,60.,89.09));
#1835=CARTESIAN_POINT('',(1.3,0.,180.));
#1836=CARTESIAN_POINT('',(1.3,45.,180.));
#1837=CARTESIAN_POINT('',(1.3,0.,178.18));
#1838=CARTESIAN_POINT('',(1.3,0.,89.09));
#1839=CARTESIAN_POINT('',(1.3,60.,178.18));
#1840=CARTESIAN_POINT('',(1.3,0.,90.92));
#1841=CARTESIAN_POINT('',(1.3,60.,90.92));
#1842=CARTESIAN_POINT('',(1.3,0.,89.08));
#1843=CARTESIAN_POINT('',(1.3,0.,44.54));
#1844=CARTESIAN_POINT('',(1.3,60.,89.08));
#1845=CARTESIAN_POINT('',(1.3,0.,1.82));
#1846=CARTESIAN_POINT('',(1.3,60.,1.82));
#1847=CARTESIAN_POINT('',(1.3,0.,0.));
#1848=CARTESIAN_POINT('',(1.3,0.,0.));
#1849=CARTESIAN_POINT('',(1.3,60.,0.));
#1850=CARTESIAN_POINT('',(1.3,45.,0.));
#1851=CARTESIAN_POINT('',(1.3,60.,1.82));
#1852=CARTESIAN_POINT('',(1.3,60.,0.));
#1853=CARTESIAN_POINT('',(1.3,60.,1.82));
#1854=CARTESIAN_POINT('',(1.3,60.,89.08));
#1855=CARTESIAN_POINT('',(1.3,60.,89.08));
#1856=CARTESIAN_POINT('',(1.3,60.,90.92));
#1857=CARTESIAN_POINT('',(1.3,60.,44.54));
#1858=CARTESIAN_POINT('',(1.3,60.,90.92));
#1859=CARTESIAN_POINT('Origin',(1.555,30.,178.18));
#1860=CARTESIAN_POINT('',(1.8,0.,178.18));
#1861=CARTESIAN_POINT('',(0.7775,0.,178.18));
#1862=CARTESIAN_POINT('',(1.8,15.,178.18));
#1863=CARTESIAN_POINT('Origin',(1.555,30.,178.18));
#1864=CARTESIAN_POINT('',(1.8,60.,178.18));
#1865=CARTESIAN_POINT('',(1.8,15.,178.18));
#1866=CARTESIAN_POINT('',(1.6775,60.,178.18));
#1867=CARTESIAN_POINT('Origin',(1.8,0.,0.));
#1868=CARTESIAN_POINT('',(1.8,0.,90.92));
#1869=CARTESIAN_POINT('',(1.8,0.,0.));
#1870=CARTESIAN_POINT('',(1.8,15.,90.92));
#1871=CARTESIAN_POINT('Origin',(1.8,0.,0.));
#1872=CARTESIAN_POINT('',(1.8,60.,90.92));
#1873=CARTESIAN_POINT('',(1.8,15.,90.92));
#1874=CARTESIAN_POINT('',(1.8,60.,0.));
#1875=CARTESIAN_POINT('Origin',(1.555,30.,90.92));
#1876=CARTESIAN_POINT('',(0.7775,0.,90.92));
#1877=CARTESIAN_POINT('Origin',(1.555,30.,90.92));
#1878=CARTESIAN_POINT('',(1.6775,60.,90.92));
#1879=CARTESIAN_POINT('Origin',(1.555,30.,89.08));
#1880=CARTESIAN_POINT('',(1.8,0.,89.08));
#1881=CARTESIAN_POINT('',(0.7775,0.,89.08));
#1882=CARTESIAN_POINT('',(1.8,15.,89.08));
#1883=CARTESIAN_POINT('Origin',(1.555,30.,89.08));
#1884=CARTESIAN_POINT('',(1.8,60.,89.08));
#1885=CARTESIAN_POINT('',(1.8,15.,89.08));
#1886=CARTESIAN_POINT('',(1.6775,60.,89.08));
#1887=CARTESIAN_POINT('Origin',(1.8,0.,0.));
#1888=CARTESIAN_POINT('',(1.8,0.,1.82));
#1889=CARTESIAN_POINT('',(1.8,0.,0.));
#1890=CARTESIAN_POINT('',(1.8,15.,1.82));
#1891=CARTESIAN_POINT('Origin',(1.8,0.,0.));
#1892=CARTESIAN_POINT('',(1.8,60.,1.82));
#1893=CARTESIAN_POINT('',(1.8,15.,1.82));
#1894=CARTESIAN_POINT('',(1.8,60.,0.));
#1895=CARTESIAN_POINT('Origin',(1.555,30.,1.82));
#1896=CARTESIAN_POINT('',(0.7775,0.,1.82));
#1897=CARTESIAN_POINT('Origin',(1.555,30.,1.82));
#1898=CARTESIAN_POINT('',(1.6775,60.,1.82));
#1899=CARTESIAN_POINT('Origin',(1.8,60.,0.));
#1900=CARTESIAN_POINT('',(0.,60.,0.));
#1901=CARTESIAN_POINT('',(1.8,60.,0.));
#1902=CARTESIAN_POINT('',(0.,60.,180.));
#1903=CARTESIAN_POINT('',(0.,60.,0.));
#1904=CARTESIAN_POINT('',(1.8,60.,180.));
#1905=CARTESIAN_POINT('Origin',(0.9,30.,0.));
#1906=CARTESIAN_POINT('',(0.,0.,0.));
#1907=CARTESIAN_POINT('',(0.,0.,0.));
#1908=CARTESIAN_POINT('',(0.,60.,0.));
#1909=CARTESIAN_POINT('Origin',(0.,0.,0.));
#1910=CARTESIAN_POINT('',(0.,0.,180.));
#1911=CARTESIAN_POINT('',(0.,0.,180.));
#1912=CARTESIAN_POINT('',(0.,0.,0.));
#1913=CARTESIAN_POINT('Origin',(0.,60.,0.));
#1914=CARTESIAN_POINT('',(0.,60.,180.));
#1915=CARTESIAN_POINT('Origin',(0.9,30.,180.));
#1916=CARTESIAN_POINT('',(0.,0.,0.));
#1917=CARTESIAN_POINT('Origin',(0.,58.18,1.3));
#1918=CARTESIAN_POINT('',(47.36,58.18,1.8));
#1919=CARTESIAN_POINT('',(0.,58.18,1.8));
#1920=CARTESIAN_POINT('',(11.84,58.18,1.8));
#1921=CARTESIAN_POINT('',(47.36,58.18,1.3));
#1922=CARTESIAN_POINT('',(47.36,58.18,0.65));
#1923=CARTESIAN_POINT('',(0.,58.18,1.3));
#1924=CARTESIAN_POINT('',(0.,58.18,1.3));
#1925=CARTESIAN_POINT('',(0.,58.18,0.65));
#1926=CARTESIAN_POINT('Origin',(47.36,58.82,1.3));
#1927=CARTESIAN_POINT('',(0.,58.82,1.8));
#1928=CARTESIAN_POINT('',(47.36,58.82,1.8));
#1929=CARTESIAN_POINT('',(35.52,58.82,1.8));
#1930=CARTESIAN_POINT('',(0.,58.82,1.3));
#1931=CARTESIAN_POINT('',(0.,58.82,0.65));
#1932=CARTESIAN_POINT('',(47.36,58.82,1.3));
#1933=CARTESIAN_POINT('',(47.36,58.82,1.3));
#1934=CARTESIAN_POINT('',(47.36,58.82,0.65));
#1935=CARTESIAN_POINT('Origin',(23.68,58.5,1.3));
#1936=CARTESIAN_POINT('',(0.,59.25,1.3));
#1937=CARTESIAN_POINT('',(47.36,29.25,1.3));
#1938=CARTESIAN_POINT('Origin',(47.36,0.,0.));
#1939=CARTESIAN_POINT('',(47.36,0.,1.8));
#1940=CARTESIAN_POINT('',(47.36,0.,1.8));
#1941=CARTESIAN_POINT('',(47.36,0.,0.));
#1942=CARTESIAN_POINT('',(47.36,0.,0.));
#1943=CARTESIAN_POINT('',(47.36,60.,0.));
#1944=CARTESIAN_POINT('',(47.36,0.,0.));
#1945=CARTESIAN_POINT('',(47.36,60.,1.8));
#1946=CARTESIAN_POINT('',(47.36,60.,0.));
#1947=CARTESIAN_POINT('',(47.36,0.,1.8));
#1948=CARTESIAN_POINT('Origin',(23.68,30.,1.8));
#1949=CARTESIAN_POINT('',(0.,0.,1.8));
#1950=CARTESIAN_POINT('',(0.,60.,1.8));
#1951=CARTESIAN_POINT('',(0.,0.,1.8));
#1952=CARTESIAN_POINT('Origin',(47.36,60.,0.));
#1953=CARTESIAN_POINT('',(0.,60.,0.));
#1954=CARTESIAN_POINT('',(47.36,60.,0.));
#1955=CARTESIAN_POINT('',(0.,60.,1.8));
#1956=CARTESIAN_POINT('',(0.,60.,0.));
#1957=CARTESIAN_POINT('',(47.36,60.,1.8));
#1958=CARTESIAN_POINT('Origin',(0.,0.,0.));
#1959=CARTESIAN_POINT('',(0.,0.,0.));
#1960=CARTESIAN_POINT('',(0.,0.,0.));
#1961=CARTESIAN_POINT('',(0.,0.,0.));
#1962=CARTESIAN_POINT('Origin',(0.,60.,0.));
#1963=CARTESIAN_POINT('',(0.,60.,1.8));
#1964=CARTESIAN_POINT('',(0.,60.,0.));
#1965=CARTESIAN_POINT('Origin',(23.68,30.,1.8));
#1966=CARTESIAN_POINT('Origin',(23.68,30.,0.));
#1967=CARTESIAN_POINT('',(0.,0.,0.));
#1968=CARTESIAN_POINT('Origin',(47.36,0.6,0.));
#1969=CARTESIAN_POINT('',(47.36,0.6,0.));
#1970=CARTESIAN_POINT('',(0.,0.6,0.));
#1971=CARTESIAN_POINT('',(47.36,0.6,0.));
#1972=CARTESIAN_POINT('',(0.,0.6,177.36));
#1973=CARTESIAN_POINT('',(0.,0.6,0.));
#1974=CARTESIAN_POINT('',(47.36,0.6,177.36));
#1975=CARTESIAN_POINT('',(47.36,0.6,177.36));
#1976=CARTESIAN_POINT('',(47.36,0.6,0.));
#1977=CARTESIAN_POINT('Origin',(47.36,0.,0.));
#1978=CARTESIAN_POINT('',(47.36,0.,0.));
#1979=CARTESIAN_POINT('',(47.36,0.,0.));
#1980=CARTESIAN_POINT('',(47.36,0.,177.36));
#1981=CARTESIAN_POINT('',(47.36,0.,177.36));
#1982=CARTESIAN_POINT('',(47.36,0.,0.));
#1983=CARTESIAN_POINT('Origin',(0.,0.,0.));
#1984=CARTESIAN_POINT('',(0.,0.,0.));
#1985=CARTESIAN_POINT('',(0.,0.,0.));
#1986=CARTESIAN_POINT('',(0.,0.,177.36));
#1987=CARTESIAN_POINT('',(0.,0.,177.36));
#1988=CARTESIAN_POINT('',(0.,0.,0.));
#1989=CARTESIAN_POINT('Origin',(0.,0.6,0.));
#1990=CARTESIAN_POINT('',(0.,0.6,0.));
#1991=CARTESIAN_POINT('',(0.,0.6,177.36));
#1992=CARTESIAN_POINT('Origin',(23.68,0.3,177.36));
#1993=CARTESIAN_POINT('Origin',(23.68,0.3,0.));
#1994=CARTESIAN_POINT('',(0.,0.,0.));
#1995=CARTESIAN_POINT('Origin',(47.36,57.6,0.));
#1996=CARTESIAN_POINT('',(47.36,57.6,0.));
#1997=CARTESIAN_POINT('',(0.,57.6,0.));
#1998=CARTESIAN_POINT('',(47.36,57.6,0.));
#1999=CARTESIAN_POINT('',(0.,57.6,1.8));
#2000=CARTESIAN_POINT('',(0.,57.6,0.));
#2001=CARTESIAN_POINT('',(47.36,57.6,1.8));
#2002=CARTESIAN_POINT('',(47.36,57.6,1.8));
#2003=CARTESIAN_POINT('',(47.36,57.6,0.));
#2004=CARTESIAN_POINT('Origin',(47.36,0.6,0.));
#2005=CARTESIAN_POINT('',(47.36,0.6,0.));
#2006=CARTESIAN_POINT('',(47.36,0.6,0.));
#2007=CARTESIAN_POINT('',(47.36,0.600000000000001,1.8));
#2008=CARTESIAN_POINT('',(47.36,0.6,1.8));
#2009=CARTESIAN_POINT('',(47.36,0.6,0.));
#2010=CARTESIAN_POINT('Origin',(0.,0.6,0.));
#2011=CARTESIAN_POINT('',(0.,0.600000000000001,0.));
#2012=CARTESIAN_POINT('',(0.,0.6,0.));
#2013=CARTESIAN_POINT('',(0.,0.600000000000001,1.8));
#2014=CARTESIAN_POINT('',(0.,0.6,1.8));
#2015=CARTESIAN_POINT('',(0.,0.600000000000001,0.));
#2016=CARTESIAN_POINT('Origin',(0.,57.6,0.));
#2017=CARTESIAN_POINT('',(0.,57.6,0.));
#2018=CARTESIAN_POINT('',(0.,57.6,1.8));
#2019=CARTESIAN_POINT('Origin',(23.68,29.1,1.8));
#2020=CARTESIAN_POINT('Origin',(23.68,29.1,0.));
#2021=CARTESIAN_POINT('',(0.,0.,0.));
#2022=CARTESIAN_POINT('Origin',(0.,0.,46.36));
#2023=CARTESIAN_POINT('',(-0.6,-7.34788079488412E-17,46.96));
#2024=CARTESIAN_POINT('Origin',(0.,0.,46.96));
#2025=CARTESIAN_POINT('',(-0.6,-7.34788079488412E-17,46.36));
#2026=CARTESIAN_POINT('',(-0.6,-7.34788079488412E-17,46.36));
#2027=CARTESIAN_POINT('Origin',(0.,0.,46.36));
#2028=CARTESIAN_POINT('Origin',(0.,0.,46.96));
#2029=CARTESIAN_POINT('Origin',(0.,0.,-0.6));
#2030=CARTESIAN_POINT('',(-0.6,-7.34788079488412E-17,0.));
#2031=CARTESIAN_POINT('Origin',(0.,0.,0.));
#2032=CARTESIAN_POINT('',(-0.6,-7.34788079488412E-17,-0.6));
#2033=CARTESIAN_POINT('',(-0.6,-7.34788079488412E-17,-0.6));
#2034=CARTESIAN_POINT('Origin',(0.,0.,-0.6));
#2035=CARTESIAN_POINT('Origin',(0.,0.,-0.6));
#2036=CARTESIAN_POINT('Origin',(0.,0.,0.));
#2037=CARTESIAN_POINT('',(-1.25,-1.53080849893419E-16,46.36));
#2038=CARTESIAN_POINT('Origin',(0.,0.,46.36));
#2039=CARTESIAN_POINT('',(-1.25,-1.53080849893419E-16,0.));
#2040=CARTESIAN_POINT('',(-1.25,-1.53080849893419E-16,0.));
#2041=CARTESIAN_POINT('Origin',(0.,0.,0.));
#2042=CARTESIAN_POINT('Origin',(0.,0.,46.36));
#2043=CARTESIAN_POINT('Origin',(0.,0.,0.));
#2044=CARTESIAN_POINT('',(0.,0.,0.));
#2045=CARTESIAN_POINT('Origin',(0.,0.,0.));
#2046=CARTESIAN_POINT('',(-0.4,-4.89858719658941E-17,2.8));
#2047=CARTESIAN_POINT('Origin',(0.,0.,2.8));
#2048=CARTESIAN_POINT('',(-0.4,-4.89858719658941E-17,0.));
#2049=CARTESIAN_POINT('',(-0.4,-4.89858719658941E-17,0.));
#2050=CARTESIAN_POINT('Origin',(0.,0.,0.));
#2051=CARTESIAN_POINT('Origin',(0.,0.,2.8));
#2052=CARTESIAN_POINT('Origin',(0.,0.,0.));
#2053=CARTESIAN_POINT('',(0.,0.,0.));
#2054=CARTESIAN_POINT('',(1.32,0.,0.));
#2055=CARTESIAN_POINT('',(1.32,58.2,1.32));
#2056=CARTESIAN_POINT('',(1.32,0.,89.1));
#2057=CARTESIAN_POINT('',(1.82,30.,162.));
#2058=CARTESIAN_POINT('',(48.6,9.,60.));
#2059=CARTESIAN_POINT('',(50.,0.,180.));
#2060=CARTESIAN_POINT('',(48.68,0.,180.));
#2061=CARTESIAN_POINT('',(50.,0.,0.));
#2062=CARTESIAN_POINT('',(100.,0.,180.));
#2063=CARTESIAN_POINT('',(51.32,0.,0.));
#2064=CARTESIAN_POINT('',(98.68,0.,180.));
#2065=CARTESIAN_POINT('',(51.32,58.2,1.32));
#2066=CARTESIAN_POINT('',(51.32,0.,89.1));
#2067=CARTESIAN_POINT('',(51.82,30.,162.));
#2068=CARTESIAN_POINT('',(100.,0.,0.));
#2069=CARTESIAN_POINT('',(150.,0.,180.));
#2070=CARTESIAN_POINT('',(101.32,0.,0.));
#2071=CARTESIAN_POINT('',(148.68,0.,180.));
#2072=CARTESIAN_POINT('',(101.32,58.2,1.32));
#2073=CARTESIAN_POINT('',(101.32,0.,89.1));
#2074=CARTESIAN_POINT('',(101.82,30.,162.));
#2075=CARTESIAN_POINT('',(48.6,9.,120.));
#2076=CARTESIAN_POINT('',(48.6,51.,60.));
#2077=CARTESIAN_POINT('',(48.6,51.,120.));
#2078=CARTESIAN_POINT('',(98.6,9.,60.));
#2079=CARTESIAN_POINT('',(98.6,9.,120.));
#2080=CARTESIAN_POINT('',(98.6,51.,60.));
#2081=CARTESIAN_POINT('',(98.6,51.,120.));
#2082=UNCERTAINTY_MEASURE_WITH_UNIT(LENGTH_MEASURE(0.001),#2098,
'DISTANCE_ACCURACY_VALUE',
'Maximum model space distance between geometric entities at asserted c
onnectivities');
#2083=UNCERTAINTY_MEASURE_WITH_UNIT(LENGTH_MEASURE(0.001),#2098,
'DISTANCE_ACCURACY_VALUE',
'Maximum model space distance between geometric entities at asserted c
onnectivities');
#2084=UNCERTAINTY_MEASURE_WITH_UNIT(LENGTH_MEASURE(0.001),#2098,
'DISTANCE_ACCURACY_VALUE',
'Maximum model space distance between geometric entities at asserted c
onnectivities');
#2085=UNCERTAINTY_MEASURE_WITH_UNIT(LENGTH_MEASURE(0.001),#2098,
'DISTANCE_ACCURACY_VALUE',
'Maximum model space distance between geometric entities at asserted c
onnectivities');
#2086=UNCERTAINTY_MEASURE_WITH_UNIT(LENGTH_MEASURE(0.001),#2098,
'DISTANCE_ACCURACY_VALUE',
'Maximum model space distance between geometric entities at asserted c
onnectivities');
#2087=UNCERTAINTY_MEASURE_WITH_UNIT(LENGTH_MEASURE(0.001),#2098,
'DISTANCE_ACCURACY_VALUE',
'Maximum model space distance between geometric entities at asserted c
onnectivities');
#2088=UNCERTAINTY_MEASURE_WITH_UNIT(LENGTH_MEASURE(0.001),#2098,
'DISTANCE_ACCURACY_VALUE',
'Maximum model space distance between geometric entities at asserted c
onnectivities');
#2089=UNCERTAINTY_MEASURE_WITH_UNIT(LENGTH_MEASURE(0.001),#2098,
'DISTANCE_ACCURACY_VALUE',
'Maximum model space distance between geometric entities at asserted c
onnectivities');
#2090=(
GEOMETRIC_REPRESENTATION_CONTEXT(3)
GLOBAL_UNCERTAINTY_ASSIGNED_CONTEXT((#2082))
GLOBAL_UNIT_ASSIGNED_CONTEXT((#2098,#2100,#2101))
REPRESENTATION_CONTEXT('','3D')
);
#2091=(
GEOMETRIC_REPRESENTATION_CONTEXT(3)
GLOBAL_UNCERTAINTY_ASSIGNED_CONTEXT((#2083))
GLOBAL_UNIT_ASSIGNED_CONTEXT((#2098,#2100,#2101))
REPRESENTATION_CONTEXT('','3D')
);
#2092=(
GEOMETRIC_REPRESENTATION_CONTEXT(3)
GLOBAL_UNCERTAINTY_ASSIGNED_CONTEXT((#2084))
GLOBAL_UNIT_ASSIGNED_CONTEXT((#2098,#2100,#2101))
REPRESENTATION_CONTEXT('','3D')
);
#2093=(
GEOMETRIC_REPRESENTATION_CONTEXT(3)
GLOBAL_UNCERTAINTY_ASSIGNED_CONTEXT((#2085))
GLOBAL_UNIT_ASSIGNED_CONTEXT((#2098,#2100,#2101))
REPRESENTATION_CONTEXT('','3D')
);
#2094=(
GEOMETRIC_REPRESENTATION_CONTEXT(3)
GLOBAL_UNCERTAINTY_ASSIGNED_CONTEXT((#2086))
GLOBAL_UNIT_ASSIGNED_CONTEXT((#2098,#2100,#2101))
REPRESENTATION_CONTEXT('','3D')
);
#2095=(
GEOMETRIC_REPRESENTATION_CONTEXT(3)
GLOBAL_UNCERTAINTY_ASSIGNED_CONTEXT((#2087))
GLOBAL_UNIT_ASSIGNED_CONTEXT((#2098,#2100,#2101))
REPRESENTATION_CONTEXT('','3D')
);
#2096=(
GEOMETRIC_REPRESENTATION_CONTEXT(3)
GLOBAL_UNCERTAINTY_ASSIGNED_CONTEXT((#2088))
GLOBAL_UNIT_ASSIGNED_CONTEXT((#2098,#2100,#2101))
REPRESENTATION_CONTEXT('','3D')
);
#2097=(
GEOMETRIC_REPRESENTATION_CONTEXT(3)
GLOBAL_UNCERTAINTY_ASSIGNED_CONTEXT((#2089))
GLOBAL_UNIT_ASSIGNED_CONTEXT((#2098,#2100,#2101))
REPRESENTATION_CONTEXT('','3D')
);
#2098=(
LENGTH_UNIT()
NAMED_UNIT(*)
SI_UNIT(.CENTI.,.METRE.)
);
#2099=(
LENGTH_UNIT()
NAMED_UNIT(*)
SI_UNIT($,.METRE.)
);
#2100=(
NAMED_UNIT(*)
PLANE_ANGLE_UNIT()
SI_UNIT($,.RADIAN.)
);
#2101=(
NAMED_UNIT(*)
SI_UNIT($,.STERADIAN.)
SOLID_ANGLE_UNIT()
);
#2102=SHAPE_DEFINITION_REPRESENTATION(#2109,#2145);
#2103=SHAPE_DEFINITION_REPRESENTATION(#2110,#2146);
#2104=SHAPE_DEFINITION_REPRESENTATION(#2111,#2147);
#2105=SHAPE_DEFINITION_REPRESENTATION(#2112,#2148);
#2106=SHAPE_DEFINITION_REPRESENTATION(#2113,#2149);
#2107=SHAPE_DEFINITION_REPRESENTATION(#2114,#2150);
#2108=SHAPE_DEFINITION_REPRESENTATION(#2115,#2151);
#2109=PRODUCT_DEFINITION_SHAPE('',$,#2153);
#2110=PRODUCT_DEFINITION_SHAPE('',$,#2154);
#2111=PRODUCT_DEFINITION_SHAPE('',$,#2155);
#2112=PRODUCT_DEFINITION_SHAPE('',$,#2156);
#2113=PRODUCT_DEFINITION_SHAPE('',$,#2157);
#2114=PRODUCT_DEFINITION_SHAPE('',$,#2158);
#2115=PRODUCT_DEFINITION_SHAPE('',$,#2159);
#2116=PRODUCT_DEFINITION_SHAPE($,$,#98);
#2117=PRODUCT_DEFINITION_SHAPE($,$,#99);
#2118=PRODUCT_DEFINITION_SHAPE($,$,#100);
#2119=PRODUCT_DEFINITION_SHAPE($,$,#101);
#2120=PRODUCT_DEFINITION_SHAPE($,$,#102);
#2121=PRODUCT_DEFINITION_SHAPE($,$,#103);
#2122=PRODUCT_DEFINITION_SHAPE($,$,#104);
#2123=PRODUCT_DEFINITION_SHAPE($,$,#105);
#2124=PRODUCT_DEFINITION_SHAPE($,$,#106);
#2125=PRODUCT_DEFINITION_SHAPE($,$,#107);
#2126=PRODUCT_DEFINITION_SHAPE($,$,#108);
#2127=PRODUCT_DEFINITION_SHAPE($,$,#109);
#2128=PRODUCT_DEFINITION_SHAPE($,$,#110);
#2129=PRODUCT_DEFINITION_SHAPE($,$,#111);
#2130=PRODUCT_DEFINITION_SHAPE($,$,#112);
#2131=PRODUCT_DEFINITION_SHAPE($,$,#113);
#2132=PRODUCT_DEFINITION_SHAPE($,$,#114);
#2133=PRODUCT_DEFINITION_SHAPE($,$,#115);
#2134=PRODUCT_DEFINITION_SHAPE($,$,#116);
#2135=PRODUCT_DEFINITION_SHAPE($,$,#117);
#2136=PRODUCT_DEFINITION_SHAPE($,$,#118);
#2137=PRODUCT_DEFINITION_SHAPE($,$,#119);
#2138=PRODUCT_DEFINITION_SHAPE($,$,#120);
#2139=PRODUCT_DEFINITION_SHAPE($,$,#121);
#2140=PRODUCT_DEFINITION_SHAPE($,$,#122);
#2141=PRODUCT_DEFINITION_SHAPE($,$,#123);
#2142=PRODUCT_DEFINITION_SHAPE($,$,#124);
#2143=PRODUCT_DEFINITION_SHAPE($,$,#125);
#2144=PRODUCT_DEFINITION_SHAPE($,$,#126);
#2145=SHAPE_REPRESENTATION('',(#1266,#1359,#1360,#1361,#1362,#1363,#1364,
#1365,#1366,#1367,#1368,#1369,#1370,#1371,#1372,#1373,#1374,#1375,#1376,
#1377,#1378,#1379,#1380,#1381,#1382,#1383,#1384,#1385,#1386,#1387),#2090);
#2146=SHAPE_REPRESENTATION('',(#1267),#2091);
#2147=SHAPE_REPRESENTATION('',(#1314),#2092);
#2148=SHAPE_REPRESENTATION('',(#1325),#2093);
#2149=SHAPE_REPRESENTATION('',(#1332),#2094);
#2150=SHAPE_REPRESENTATION('',(#1339),#2095);
#2151=SHAPE_REPRESENTATION('',(#1353),#2096);
#2152=PRODUCT_DEFINITION_CONTEXT('part definition',#2175,'design');
#2153=PRODUCT_DEFINITION('TAS-021','TAS-021',#2160,#2152);
#2154=PRODUCT_DEFINITION('Universal side panel','Universal side panel',
#2161,#2152);
#2155=PRODUCT_DEFINITION('Horizontal closure panel',
'Horizontal closure panel',#2162,#2152);
#2156=PRODUCT_DEFINITION('Captured back panel','Captured back panel',#2163,
#2152);
#2157=PRODUCT_DEFINITION('Fixed shelf','Fixed shelf',#2164,#2152);
#2158=PRODUCT_DEFINITION('Hanging rail','Hanging rail',#2165,#2152);
#2159=PRODUCT_DEFINITION('Bay coupling dowel','Bay coupling dowel',#2166,
#2152);
#2160=PRODUCT_DEFINITION_FORMATION('',$,#2177);
#2161=PRODUCT_DEFINITION_FORMATION('',$,#2178);
#2162=PRODUCT_DEFINITION_FORMATION('',$,#2179);
#2163=PRODUCT_DEFINITION_FORMATION('',$,#2180);
#2164=PRODUCT_DEFINITION_FORMATION('',$,#2181);
#2165=PRODUCT_DEFINITION_FORMATION('',$,#2182);
#2166=PRODUCT_DEFINITION_FORMATION('',$,#2183);
#2167=PRODUCT_RELATED_PRODUCT_CATEGORY('TAS-021','TAS-021',(#2177));
#2168=PRODUCT_RELATED_PRODUCT_CATEGORY('Universal side panel',
'Universal side panel',(#2178));
#2169=PRODUCT_RELATED_PRODUCT_CATEGORY('Horizontal closure panel',
'Horizontal closure panel',(#2179));
#2170=PRODUCT_RELATED_PRODUCT_CATEGORY('Captured back panel',
'Captured back panel',(#2180));
#2171=PRODUCT_RELATED_PRODUCT_CATEGORY('Fixed shelf','Fixed shelf',(#2181));
#2172=PRODUCT_RELATED_PRODUCT_CATEGORY('Hanging rail','Hanging rail',(#2182));
#2173=PRODUCT_RELATED_PRODUCT_CATEGORY('Bay coupling dowel',
'Bay coupling dowel',(#2183));
#2174=APPLICATION_PROTOCOL_DEFINITION('international standard',
'automotive_design',2009,#2175);
#2175=APPLICATION_CONTEXT(
'Core Data for Automotive Mechanical Design Process');
#2176=PRODUCT_CONTEXT('part definition',#2175,'mechanical');
#2177=PRODUCT('TAS-021','TAS-021',$,(#2176));
#2178=PRODUCT('Universal side panel','Universal side panel',$,(#2176));
#2179=PRODUCT('Horizontal closure panel','Horizontal closure panel',$,(#2176));
#2180=PRODUCT('Captured back panel','Captured back panel',$,(#2176));
#2181=PRODUCT('Fixed shelf','Fixed shelf',$,(#2176));
#2182=PRODUCT('Hanging rail','Hanging rail',$,(#2176));
#2183=PRODUCT('Bay coupling dowel','Bay coupling dowel',$,(#2176));
#2184=PRESENTATION_STYLE_ASSIGNMENT((#2191));
#2185=PRESENTATION_STYLE_ASSIGNMENT((#2192));
#2186=PRESENTATION_STYLE_ASSIGNMENT((#2193));
#2187=PRESENTATION_STYLE_ASSIGNMENT((#2194));
#2188=PRESENTATION_STYLE_ASSIGNMENT((#2195));
#2189=PRESENTATION_STYLE_ASSIGNMENT((#2196));
#2190=PRESENTATION_STYLE_ASSIGNMENT((#2197));
#2191=SURFACE_STYLE_USAGE(.BOTH.,#2198);
#2192=SURFACE_STYLE_USAGE(.BOTH.,#2199);
#2193=SURFACE_STYLE_USAGE(.BOTH.,#2200);
#2194=SURFACE_STYLE_USAGE(.BOTH.,#2201);
#2195=SURFACE_STYLE_USAGE(.BOTH.,#2202);
#2196=SURFACE_STYLE_USAGE(.BOTH.,#2203);
#2197=SURFACE_STYLE_USAGE(.BOTH.,#2204);
#2198=SURFACE_SIDE_STYLE('',(#2205));
#2199=SURFACE_SIDE_STYLE('',(#2206));
#2200=SURFACE_SIDE_STYLE('',(#2207));
#2201=SURFACE_SIDE_STYLE('',(#2208));
#2202=SURFACE_SIDE_STYLE('',(#2209));
#2203=SURFACE_SIDE_STYLE('',(#2210));
#2204=SURFACE_SIDE_STYLE('',(#2211));
#2205=SURFACE_STYLE_FILL_AREA(#2212);
#2206=SURFACE_STYLE_FILL_AREA(#2213);
#2207=SURFACE_STYLE_FILL_AREA(#2214);
#2208=SURFACE_STYLE_FILL_AREA(#2215);
#2209=SURFACE_STYLE_FILL_AREA(#2216);
#2210=SURFACE_STYLE_FILL_AREA(#2217);
#2211=SURFACE_STYLE_FILL_AREA(#2218);
#2212=FILL_AREA_STYLE('Steel - Satin',(#2219));
#2213=FILL_AREA_STYLE('Universal side panel finish',(#2220));
#2214=FILL_AREA_STYLE('Horizontal closure panel finish',(#2221));
#2215=FILL_AREA_STYLE('Captured back panel finish',(#2222));
#2216=FILL_AREA_STYLE('Fixed shelf finish',(#2223));
#2217=FILL_AREA_STYLE('Hanging rail finish',(#2224));
#2218=FILL_AREA_STYLE('Bay coupling dowel finish',(#2225));
#2219=FILL_AREA_STYLE_COLOUR('Steel - Satin',#2226);
#2220=FILL_AREA_STYLE_COLOUR('Universal side panel finish',#2227);
#2221=FILL_AREA_STYLE_COLOUR('Horizontal closure panel finish',#2228);
#2222=FILL_AREA_STYLE_COLOUR('Captured back panel finish',#2229);
#2223=FILL_AREA_STYLE_COLOUR('Fixed shelf finish',#2230);
#2224=FILL_AREA_STYLE_COLOUR('Hanging rail finish',#2231);
#2225=FILL_AREA_STYLE_COLOUR('Bay coupling dowel finish',#2232);
#2226=COLOUR_RGB('Steel - Satin',0.627450980392157,0.627450980392157,0.627450980392157);
#2227=COLOUR_RGB('Universal side panel finish',0.0941176470588235,0.231372549019608,
0.431372549019608);
#2228=COLOUR_RGB('Horizontal closure panel finish',0.662745098039216,0.823529411764706,
0.917647058823529);
#2229=COLOUR_RGB('Captured back panel finish',0.607843137254902,0.647058823529412,
0.701960784313725);
#2230=COLOUR_RGB('Fixed shelf finish',0.274509803921569,0.6,0.8);
#2231=COLOUR_RGB('Hanging rail finish',0.607843137254902,0.647058823529412,
0.701960784313725);
#2232=COLOUR_RGB('Bay coupling dowel finish',0.43921568627451,0.47843137254902,
0.52156862745098);
ENDSEC;
END-ISO-10303-21;
